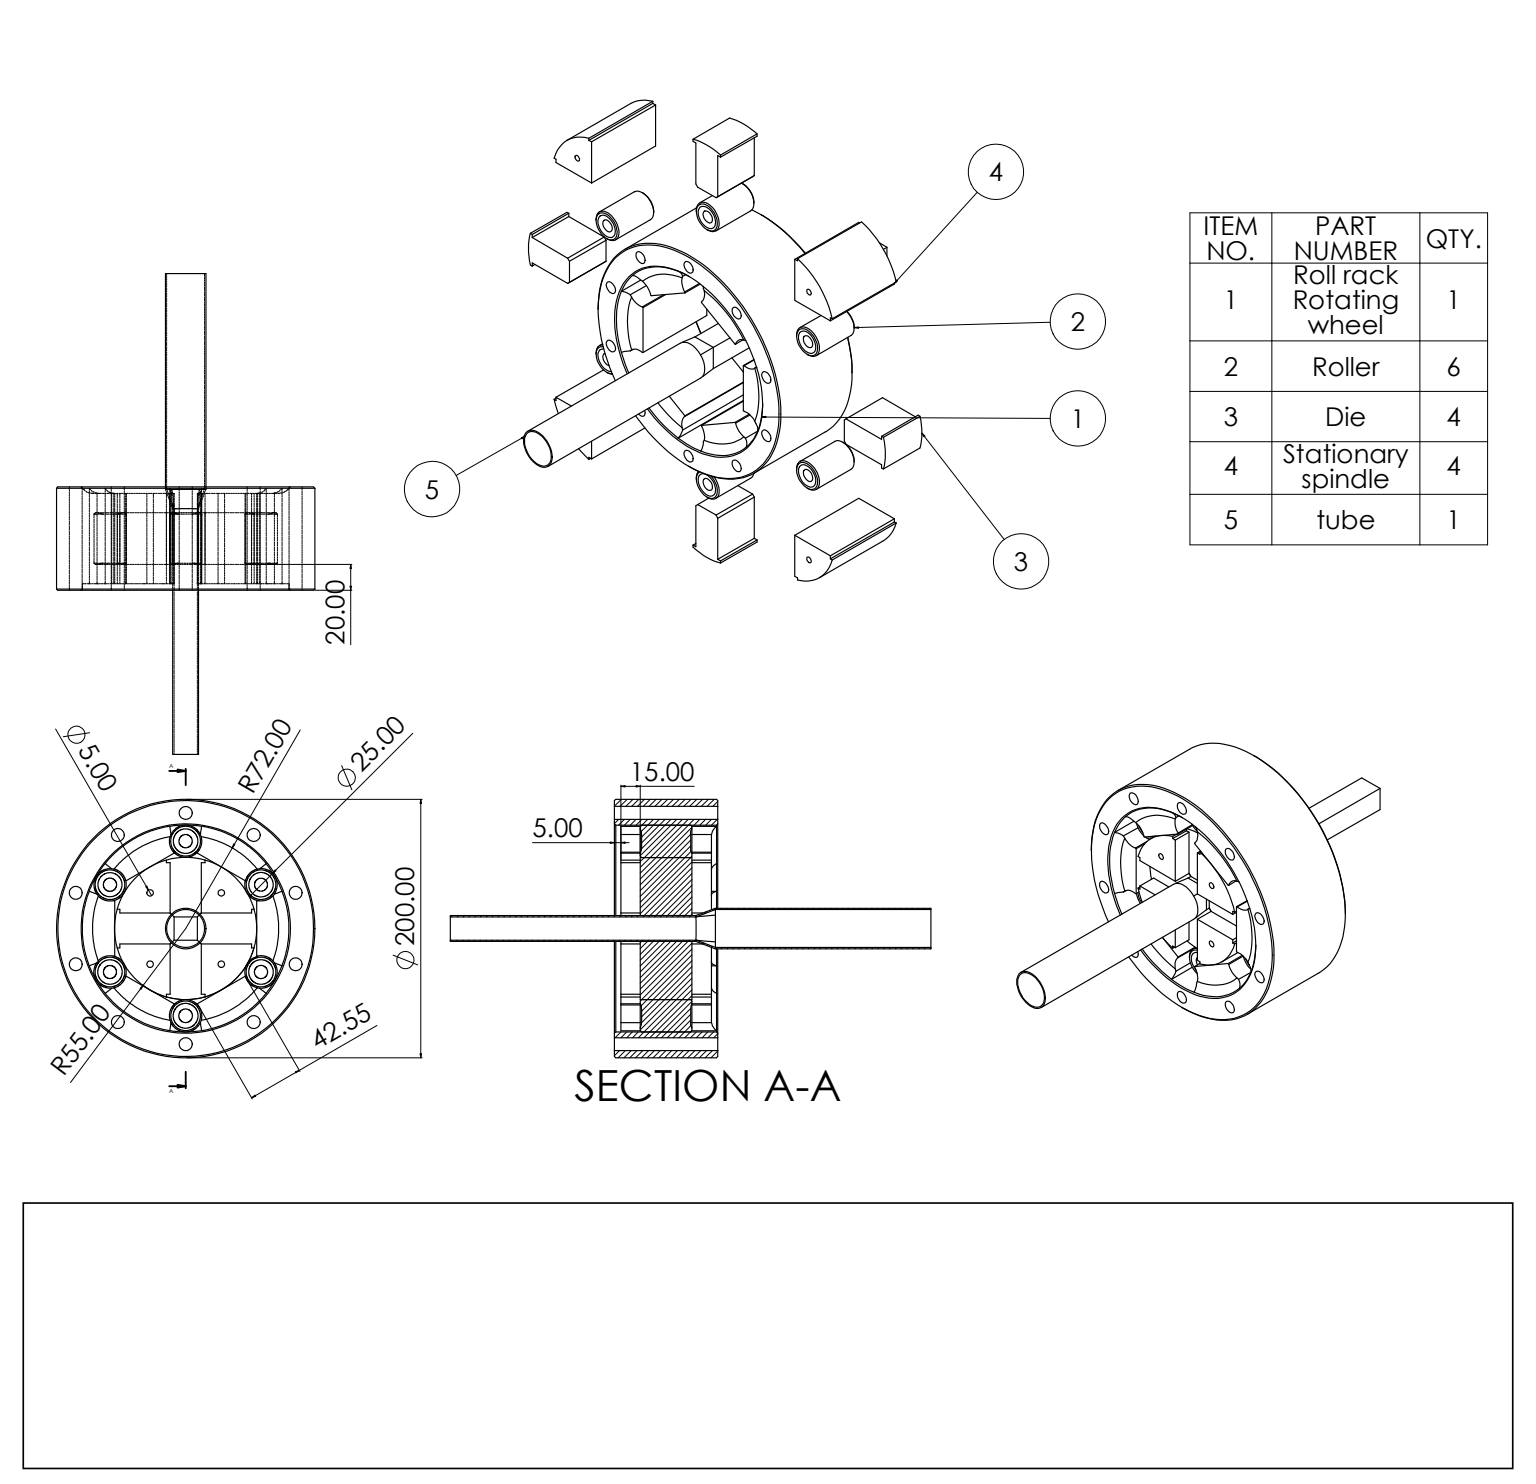
ISO-10303-21;
HEADER;
FILE_DESCRIPTION (('STEP AP214'),
    '1' );
FILE_NAME ('MAS-319',
    '2026-10-25T19:19:31',
    ( '' ),
    ( '' ),
    'SwSTEP 2.0',
    'SolidWorks 2025',
    '' );
FILE_SCHEMA (( 'AUTOMOTIVE_DESIGN' ));
ENDSEC;

DATA;
#1 = FACE_OUTER_BOUND ( 'NONE', #2199, .T. ) ;
#2 = AXIS2_PLACEMENT_3D ( 'NONE', #924, #2806, #4329 ) ;
#3 = CARTESIAN_POINT ( 'NONE',  ( 6.000509662810415534, -9.000000000000001776, 23.13502399099470708 ) ) ;
#4 = DIRECTION ( 'NONE',  ( 1.000000000000000000, 1.776356839400250465E-15, 0.000000000000000000 ) ) ;
#5 = ORIENTED_EDGE ( 'NONE', *, *, #469, .T. ) ;
#6 = LINE ( 'NONE', #939, #4428 ) ;
#7 = CYLINDRICAL_SURFACE ( 'NONE', #5135, 14.67638808697554964 ) ;
#8 = ADVANCED_FACE ( 'NONE', ( #6005 ), #1741, .T. ) ;
#9 = EDGE_CURVE ( 'NONE', #3175, #2261, #1933, .T. ) ;
#10 =( NAMED_UNIT ( * ) SI_UNIT ( $, .STERADIAN. ) SOLID_ANGLE_UNIT ( ) );
#11 = EDGE_LOOP ( 'NONE', ( #620, #96, #4571, #312 ) ) ;
#12 = DIRECTION ( 'NONE',  ( 0.6273063437270283149, 0.7787725926866119197, -0.000000000000000000 ) ) ;
#13 = PRODUCT_DEFINITION_SHAPE ( 'NONE', 'NONE',  #6150 ) ;
#14 = CARTESIAN_POINT ( 'NONE',  ( 4.154428044945162490, -8.963431230391421423, 23.04275563843252783 ) ) ;
#15 = VERTEX_POINT ( 'NONE', #3832 ) ;
#16 = ORIENTED_EDGE ( 'NONE', *, *, #1748, .F. ) ;
#17 = LINE ( 'NONE', #2869, #5066 ) ;
#18 = PLANE ( 'NONE',  #4619 ) ;
#19 =( NAMED_UNIT ( * ) SI_UNIT ( $, .STERADIAN. ) SOLID_ANGLE_UNIT ( ) );
#20 = DIRECTION ( 'NONE',  ( 2.553512956637860437E-15, -1.000000000000000000, 1.499031448860895265E-16 ) ) ;
#21 = EDGE_CURVE ( 'NONE', #4952, #1308, #564, .T. ) ;
#22 = CARTESIAN_POINT ( 'NONE',  ( 0.000000000000000000, 0.000000000000000000, -35.00000000000000000 ) ) ;
#23 = DIRECTION ( 'NONE',  ( 0.000000000000000000, -1.000000000000000000, 0.000000000000000000 ) ) ;
#24 = ORIENTED_EDGE ( 'NONE', *, *, #3439, .T. ) ;
#25 = CARTESIAN_POINT ( 'NONE',  ( 4.399209358691966720, 10.59950146047779995, 28.13666863833444154 ) ) ;
#26 = CARTESIAN_POINT ( 'NONE',  ( -0.8333333333332849646, 10.00000000000000000, 23.00000000000000355 ) ) ;
#27 = FACE_OUTER_BOUND ( 'NONE', #743, .T. ) ;
#28 = ORIENTED_EDGE ( 'NONE', *, *, #3600, .T. ) ;
#29 = CARTESIAN_POINT ( 'NONE',  ( -27.50000000000000355, -47.63139720814412215, 35.00000000000000000 ) ) ;
#30 = CARTESIAN_POINT ( 'NONE',  ( 0.000000000000000000, -67.50000000000000000, 35.00000000000000000 ) ) ;
#31 = CARTESIAN_POINT ( 'NONE',  ( -9.557272410707511767, 9.557272410707513544, 28.03893107092313031 ) ) ;
#32 = CARTESIAN_POINT ( 'NONE',  ( -68.69027832784050247, 26.57196568621489163, 35.13717928826310555 ) ) ;
#33 = ORIENTED_EDGE ( 'NONE', *, *, #1361, .F. ) ;
#34 = CARTESIAN_POINT ( 'NONE',  ( 0.000000000000000000, 0.000000000000000000, -39.00000000000002842 ) ) ;
#35 = DIRECTION ( 'NONE',  ( 0.000000000000000000, -1.000000000000000000, 0.000000000000000000 ) ) ;
#36 = DIRECTION ( 'NONE',  ( -0.000000000000000000, -0.000000000000000000, -1.000000000000000000 ) ) ;
#37 = VERTEX_POINT ( 'NONE', #2442 ) ;
#38 = CARTESIAN_POINT ( 'NONE',  ( 10.37777353962609972, -10.37777353962564852, 38.05103295300747845 ) ) ;
#39 = CARTESIAN_POINT ( 'NONE',  ( 5.954763795926170999, -9.638809746143389035, 25.54536317066256856 ) ) ;
#40 = APPLICATION_CONTEXT ( 'automotive_design' ) ;
#41 = EDGE_CURVE ( 'NONE', #1178, #2811, #1439, .T. ) ;
#42 = ORIENTED_EDGE ( 'NONE', *, *, #5266, .F. ) ;
#43 = ORIENTED_EDGE ( 'NONE', *, *, #3427, .F. ) ;
#44 = DIRECTION ( 'NONE',  ( 1.000000000000000000, 0.000000000000000000, 0.000000000000000000 ) ) ;
#45 = LINE ( 'NONE', #2928, #381 ) ;
#46 = DIRECTION ( 'NONE',  ( 5.551115123125782702E-17, 2.775557561562891351E-17, 1.000000000000000000 ) ) ;
#47 = CARTESIAN_POINT ( 'NONE',  ( 9.858401829237470437, -10.19494410001831142, 33.01259202755186095 ) ) ;
#48 = EDGE_CURVE ( 'NONE', #2705, #6084, #5252, .T. ) ;
#49 = ORIENTED_EDGE ( 'NONE', *, *, #1979, .T. ) ;
#50 = CARTESIAN_POINT ( 'NONE',  ( 1.902388932222473850, 12.74242197681752486, 33.26151580524048512 ) ) ;
#51 = CARTESIAN_POINT ( 'NONE',  ( 11.08488032081242380, 11.08488032081242025, 38.00000000000000000 ) ) ;
#52 = CARTESIAN_POINT ( 'NONE',  ( -85.08403291566554572, 27.64547812922971914, -40.00000000000000000 ) ) ;
#53 = AXIS2_PLACEMENT_3D ( 'NONE', #2121, #1570, #3471 ) ;
#54 = ORIENTED_EDGE ( 'NONE', *, *, #4887, .F. ) ;
#55 = DIRECTION ( 'NONE',  ( -0.000000000000000000, -0.000000000000000000, -1.000000000000000000 ) ) ;
#56 = ADVANCED_FACE ( 'NONE', ( #3401 ), #273, .T. ) ;
#57 = CARTESIAN_POINT ( 'NONE',  ( -10.12138240269938905, -10.27356722921338950, 35.55812462721154787 ) ) ;
#58 = AXIS2_PLACEMENT_3D ( 'NONE', #3243, #1826, #3726 ) ;
#59=STYLED_ITEM('',(#6177),#4119);
#60 = DIRECTION ( 'NONE',  ( -1.224646799147353207E-16, 1.000000000000000000, 0.000000000000000000 ) ) ;
#61 = PRODUCT_DEFINITION_SHAPE ( 'NONE', 'NONE',  #6146 ) ;
#62 = VECTOR ( 'NONE', #4313, 1000.000000000000000 ) ;
#63 = DIRECTION ( 'NONE',  ( 0.000000000000000000, 0.000000000000000000, -1.000000000000000000 ) ) ;
#64 = CARTESIAN_POINT ( 'NONE',  ( -3.819063922341606521, -14.20304409106748977, 38.16887386538299154 ) ) ;
#65 = AXIS2_PLACEMENT_3D ( 'NONE', #52, #3436, #1534 ) ;
#66 = ORIENTED_EDGE ( 'NONE', *, *, #1371, .T. ) ;
#67 = LINE ( 'NONE', #4284, #175 ) ;
#68 = AXIS2_PLACEMENT_3D ( 'NONE', #5525, #4167, #5643 ) ;
#69 = DIRECTION ( 'NONE',  ( -0.000000000000000000, 0.000000000000000000, 1.000000000000000000 ) ) ;
#70 = LINE ( 'NONE', #4287, #2332 ) ;
#71 = ORIENTED_EDGE ( 'NONE', *, *, #3542, .T. ) ;
#72 = LINE ( 'NONE', #3851, #3967 ) ;
#73 = AXIS2_PLACEMENT_3D ( 'NONE', #3304, #3763, #5645 ) ;
#74 = CARTESIAN_POINT ( 'NONE',  ( 3.019346778933465369, -14.42236408824967420, 38.33740271606986738 ) ) ;
#75 = MECHANICAL_DESIGN_GEOMETRIC_PRESENTATION_REPRESENTATION (  '', ( #2849 ), #6131 ) ;
#76 = ORIENTED_EDGE ( 'NONE', *, *, #3903, .F. ) ;
#77 = PRESENTATION_STYLE_ASSIGNMENT (( #649 ) ) ;
#78 = ORIENTED_EDGE ( 'NONE', *, *, #3494, .T. ) ;
#79 = DIRECTION ( 'NONE',  ( -0.000000000000000000, -0.000000000000000000, 1.000000000000000000 ) ) ;
#80 = DIRECTION ( 'NONE',  ( -0.000000000000000000, -0.000000000000000000, -1.000000000000000000 ) ) ;
#81 = CARTESIAN_POINT ( 'NONE',  ( 0.000000000000000000, 0.000000000000000000, 0.000000000000000000 ) ) ;
#82 = SHAPE_REPRESENTATION ( 'Roller', ( #73 ), #2452 ) ;
#83 = DIRECTION ( 'NONE',  ( 0.000000000000000000, 0.000000000000000000, 1.000000000000000000 ) ) ;
#84 = CARTESIAN_POINT ( 'NONE',  ( 58.45671475545002949, -33.74999999999933209, 35.00000000000000000 ) ) ;
#85 = ORIENTED_EDGE ( 'NONE', *, *, #1081, .T. ) ;
#86 = VECTOR ( 'NONE', #3244, 1000.000000000000114 ) ;
#87 = CARTESIAN_POINT ( 'NONE',  ( -1.016991241531515433, 14.74111653287705792, 38.35393095385146012 ) ) ;
#88 = CARTESIAN_POINT ( 'NONE',  ( -4.130675435985315210E-14, -1.067806758184287486E-13, -35.00000000000000000 ) ) ;
#89 = DIRECTION ( 'NONE',  ( -0.000000000000000000, -0.000000000000000000, 1.000000000000000000 ) ) ;
#90 = EDGE_CURVE ( 'NONE', #1861, #5383, #5968, .T. ) ;
#91 = ORIENTED_EDGE ( 'NONE', *, *, #553, .T. ) ;
#92 = CYLINDRICAL_SURFACE ( 'NONE', #5438, 12.50000000000000355 ) ;
#93 = CIRCLE ( 'NONE', #494, 100.0000000000000000 ) ;
#94 = DIRECTION ( 'NONE',  ( -0.000000000000000000, -0.000000000000000000, -1.000000000000000000 ) ) ;
#95 = VECTOR ( 'NONE', #4136, 1000.000000000000000 ) ;
#96 = ORIENTED_EDGE ( 'NONE', *, *, #2491, .F. ) ;
#97 = VECTOR ( 'NONE', #2993, 1000.000000000000000 ) ;
#98 = DIRECTION ( 'NONE',  ( -1.000000000000000000, 0.000000000000000000, 0.000000000000000000 ) ) ;
#99 = EDGE_CURVE ( 'NONE', #3250, #2370, #287, .T. ) ;
#100 = VECTOR ( 'NONE', #4962, 1000.000000000000000 ) ;
#101 = CARTESIAN_POINT ( 'NONE',  ( 0.000000000000000000, 67.50000000000000000, -20.00000000000000000 ) ) ;
#102 = CARTESIAN_POINT ( 'NONE',  ( 0.000000000000000000, 0.000000000000000000, 205.0000000000000568 ) ) ;
#103 = VERTEX_POINT ( 'NONE', #3026 ) ;
#104 = DIRECTION ( 'NONE',  ( 1.000000000000000000, 0.000000000000000000, 0.000000000000000000 ) ) ;
#105 = CARTESIAN_POINT ( 'NONE',  ( 0.000000000000000000, 0.000000000000000000, -20.00000000000000000 ) ) ;
#106 = CARTESIAN_POINT ( 'NONE',  ( 90.08403291566575888, -27.64547812922912939, -40.00000000000000000 ) ) ;
#107 = ORIENTED_EDGE ( 'NONE', *, *, #3615, .T. ) ;
#108 = CARTESIAN_POINT ( 'NONE',  ( 12.00000000000000000, 12.00000000000000355, 35.00000000000000000 ) ) ;
#109 = CARTESIAN_POINT ( 'NONE',  ( 6.925838250501021420, -10.16165675636470489, 28.06531976343184454 ) ) ;
#110 = ORIENTED_EDGE ( 'NONE', *, *, #2448, .F. ) ;
#111 = ORIENTED_EDGE ( 'NONE', *, *, #3009, .T. ) ;
#112 = DIRECTION ( 'NONE',  ( -1.000000000000000000, 0.000000000000000000, 0.000000000000000000 ) ) ;
#113 = LINE ( 'NONE', #4877, #5053 ) ;
#114 = DIRECTION ( 'NONE',  ( -6.989357705721002594E-18, 6.660920792866264645E-17, 1.000000000000000000 ) ) ;
#115 = CARTESIAN_POINT ( 'NONE',  ( -10.37777353962477278, -10.37777353962696303, 38.05103295300743582 ) ) ;
#116 = CARTESIAN_POINT ( 'NONE',  ( 10.38144361273100280, -10.38144361273100813, 38.10175261887127363 ) ) ;
#117 = ORIENTED_EDGE ( 'NONE', *, *, #561, .F. ) ;
#118 = PRODUCT_DEFINITION ( 'UNKNOWN', '', #4533, #1451 ) ;
#119 = ORIENTED_EDGE ( 'NONE', *, *, #3607, .F. ) ;
#120 = CARTESIAN_POINT ( 'NONE',  ( 4.273055220303958457, 9.778265677387498300, 25.59105958838677353 ) ) ;
#121 = CARTESIAN_POINT ( 'NONE',  ( 11.73806315776973719, 10.43169748385510687, 38.00000000000000000 ) ) ;
#122 = CARTESIAN_POINT ( 'NONE',  ( -13.19705249345109088, -6.492124056757525352, 38.13875458540262997 ) ) ;
#123 = ORIENTED_EDGE ( 'NONE', *, *, #596, .F. ) ;
#124 = CARTESIAN_POINT ( 'NONE',  ( 0.000000000000000000, 67.50000000000000000, -28.99999999999999645 ) ) ;
#125 = CARTESIAN_POINT ( 'NONE',  ( -11.58282027941458381, -3.645499761006322892, 30.69674202529823503 ) ) ;
#126 = ORIENTED_EDGE ( 'NONE', *, *, #1149, .F. ) ;
#127 = EDGE_CURVE ( 'NONE', #4172, #3364, #4015, .T. ) ;
#128 = EDGE_CURVE ( 'NONE', #3596, #4984, #485, .T. ) ;
#129 = CARTESIAN_POINT ( 'NONE',  ( 8.309552794738946702, -9.958856949317492990, 22.73823205004162773 ) ) ;
#130 = EDGE_CURVE ( 'NONE', #3466, #5138, #2058, .T. ) ;
#131 = CARTESIAN_POINT ( 'NONE',  ( 0.9493919581231019533, -14.67711297304296281, 38.18288466297301653 ) ) ;
#132 = VERTEX_POINT ( 'NONE', #187 ) ;
#133 = CARTESIAN_POINT ( 'NONE',  ( 6.000548030722291593, 8.999999999999994671, 23.13502304888907446 ) ) ;
#134 = CARTESIAN_POINT ( 'NONE',  ( 0.000000000000000000, 67.50000000000000000, -19.00000000000000711 ) ) ;
#135 = CARTESIAN_POINT ( 'NONE',  ( 11.82353433160363387, 71.60642589802917257, 35.00000000000000000 ) ) ;
#136 = CARTESIAN_POINT ( 'NONE',  ( -5.141101056459331353, 67.50000000000000000, -19.00000000000000000 ) ) ;
#137 = CARTESIAN_POINT ( 'NONE',  ( 8.328520801854331523, -12.11088206474084572, 38.20782360758020246 ) ) ;
#138 = EDGE_CURVE ( 'NONE', #2272, #193, #3964, .T. ) ;
#139 = ORIENTED_EDGE ( 'NONE', *, *, #5184, .F. ) ;
#140 = ORIENTED_EDGE ( 'NONE', *, *, #2807, .F. ) ;
#141 = DIRECTION ( 'NONE',  ( -1.000000000000000000, 0.000000000000000000, 0.000000000000000000 ) ) ;
#142 = DIRECTION ( 'NONE',  ( -0.4999999999999919509, -0.8660254037844432595, 0.000000000000000000 ) ) ;
#143 = DIRECTION ( 'NONE',  ( 0.8660254037844374864, 0.5000000000000018874, 0.000000000000000000 ) ) ;
#144 = CARTESIAN_POINT ( 'NONE',  ( 55.71784976887228424, -21.55374571496028224, -35.00000000000000000 ) ) ;
#145 = EDGE_LOOP ( 'NONE', ( #2402, #588 ) ) ;
#146 = CARTESIAN_POINT ( 'NONE',  ( 0.8581648076837656847, 9.928243323025451872, 25.63579099555280649 ) ) ;
#147 = CARTESIAN_POINT ( 'NONE',  ( 2.164213882025735280, 15.56315586465742484, 38.00000000000000711 ) ) ;
#148 = CARTESIAN_POINT ( 'NONE',  ( -99.00000000000005684, 0.000000000000000000, 40.00000000000000000 ) ) ;
#149 = VERTEX_POINT ( 'NONE', #4105 ) ;
#150 = DIRECTION ( 'NONE',  ( 0.000000000000000000, 0.000000000000000000, 1.000000000000000000 ) ) ;
#151 = CARTESIAN_POINT ( 'NONE',  ( -13.51119013911330491, -2.923529524533183821, 35.79437308157103814 ) ) ;
#152 = ORIENTED_EDGE ( 'NONE', *, *, #4059, .F. ) ;
#153 = CARTESIAN_POINT ( 'NONE',  ( -2.164213882025736613, -15.56315586465742484, 38.00000000000000711 ) ) ;
#154 = EDGE_CURVE ( 'NONE', #2132, #2202, #3672, .T. ) ;
#155 = CIRCLE ( 'NONE', #3811, 12.50000000000138733 ) ;
#156 = CARTESIAN_POINT ( 'NONE',  ( 8.964680801521355491, 2.491918585145397991, 23.07363600708416129 ) ) ;
#157 = CARTESIAN_POINT ( 'NONE',  ( -67.92475106770436355, 25.56373185532726566, 35.00000000000000000 ) ) ;
#158 = ORIENTED_EDGE ( 'NONE', *, *, #5715, .F. ) ;
#159 = FACE_OUTER_BOUND ( 'NONE', #3787, .T. ) ;
#160 = CIRCLE ( 'NONE', #3618, 5.000000000000004441 ) ;
#161 = APPLICATION_CONTEXT ( 'automotive_design' ) ;
#162 = CIRCLE ( 'NONE', #672, 99.00000000000005684 ) ;
#163 = LINE ( 'NONE', #3014, #5926 ) ;
#164 = EDGE_CURVE ( 'NONE', #4020, #3411, #5117, .T. ) ;
#165 = AXIS2_PLACEMENT_3D ( 'NONE', #2293, #4791, #5233 ) ;
#166 = CARTESIAN_POINT ( 'NONE',  ( -90.08403291566554572, 27.64547812922971914, 40.00000000000000000 ) ) ;
#167 = PRODUCT_DEFINITION_SHAPE ( 'NONE', 'NONE',  #6142 ) ;
#168 = CARTESIAN_POINT ( 'NONE',  ( 1.016991241531512769, -14.74111653287705792, 38.35393095385146012 ) ) ;
#169 = CIRCLE ( 'NONE', #2831, 12.49999999999999822 ) ;
#170 = AXIS2_PLACEMENT_3D ( 'NONE', #2221, #6035, #3192 ) ;
#171 = ORIENTED_EDGE ( 'NONE', *, *, #1511, .T. ) ;
#172 = FACE_OUTER_BOUND ( 'NONE', #5895, .T. ) ;
#173 = ORIENTED_EDGE ( 'NONE', *, *, #319, .F. ) ;
#174 = PLANE ( 'NONE',  #2670 ) ;
#175 = VECTOR ( 'NONE', #443, 1000.000000000000000 ) ;
#176 = B_SPLINE_CURVE_WITH_KNOTS ( 'NONE', 3,
 ( #5640, #360, #5088, #1772, #3271, #6050 ),
 .UNSPECIFIED., .F., .F.,
 ( 4, 2, 4 ),
 ( 2.991083261079382436E-05, 0.007589224902417026838, 0.01514853897222325982 ),
 .UNSPECIFIED. ) ;
#177 = DIRECTION ( 'NONE',  ( 0.000000000000000000, 0.000000000000000000, 1.000000000000000000 ) ) ;
#178 = SHAPE_DEFINITION_REPRESENTATION ( #473, #4081 ) ;
#179 = AXIS2_PLACEMENT_3D ( 'NONE', #1316, #5314, #565 ) ;
#180 = CARTESIAN_POINT ( 'NONE',  ( 8.999999999999998224, -9.999999999999998224, 23.00000000000000000 ) ) ;
#181 = EDGE_CURVE ( 'NONE', #882, #2297, #5215, .T. ) ;
#182 = DIRECTION ( 'NONE',  ( -0.000000000000000000, -0.000000000000000000, -1.000000000000000000 ) ) ;
#183 = ORIENTED_EDGE ( 'NONE', *, *, #3874, .T. ) ;
#184 = VECTOR ( 'NONE', #2953, 1000.000000000000000 ) ;
#185 = EDGE_LOOP ( 'NONE', ( #533, #4724, #4763, #1601 ) ) ;
#186 = CARTESIAN_POINT ( 'NONE',  ( 5.819377809724670669, 8.963566137365393871, 22.99383900881164067 ) ) ;
#187 = CARTESIAN_POINT ( 'NONE',  ( -11.33314185116896589, -72.77350886803867525, -35.00000000000000000 ) ) ;
#188 = FACE_OUTER_BOUND ( 'NONE', #757, .T. ) ;
#189 = AXIS2_PLACEMENT_3D ( 'NONE', #1496, #4390, #4322 ) ;
#190 = ORIENTED_EDGE ( 'NONE', *, *, #4573, .T. ) ;
#191 = DIRECTION ( 'NONE',  ( -1.000000000000000000, 0.000000000000000000, 0.000000000000000000 ) ) ;
#192 = CARTESIAN_POINT ( 'NONE',  ( -9.928243323025453648, 3.951802415609825688E-14, 25.63579099555280294 ) ) ;
#193 = VERTEX_POINT ( 'NONE', #6023 ) ;
#194 = CARTESIAN_POINT ( 'NONE',  ( -3.317157231508649495, -9.910574073276151807, 22.73823205004162773 ) ) ;
#195 = VECTOR ( 'NONE', #4584, 1000.000000000000000 ) ;
#196 = CARTESIAN_POINT ( 'NONE',  ( 13.51119013911330669, 2.923529524533184265, 35.79437308157104525 ) ) ;
#197 = AXIS2_PLACEMENT_3D ( 'NONE', #5583, #3182, #1309 ) ;
#198 = LINE ( 'NONE', #2374, #5423 ) ;
#199 = EDGE_LOOP ( 'NONE', ( #4634, #1674, #4035, #780 ) ) ;
#200 = CARTESIAN_POINT ( 'NONE',  ( -56.72666074499610289, 46.14586675604117971, 35.04915833130703362 ) ) ;
#201 = CIRCLE ( 'NONE', #4460, 80.99999999999998579 ) ;
#202 = AXIS2_PLACEMENT_3D ( 'NONE', #584, #4355, #522 ) ;
#203 = CARTESIAN_POINT ( 'NONE',  ( 0.8880320553140116369, -10.89081796499577237, 28.17941898721254645 ) ) ;
#204 = ORIENTED_EDGE ( 'NONE', *, *, #2780, .T. ) ;
#205 = DIRECTION ( 'NONE',  ( -0.000000000000000000, -0.000000000000000000, -1.000000000000000000 ) ) ;
#206 = ORIENTED_EDGE ( 'NONE', *, *, #6021, .F. ) ;
#207 = CARTESIAN_POINT ( 'NONE',  ( 14.30354638250598498, 3.321916882804190951, 38.17191617598167852 ) ) ;
#208 = EDGE_CURVE ( 'NONE', #3788, #4471, #2464, .T. ) ;
#209 = ADVANCED_FACE ( 'NONE', ( #3211 ), #1827, .F. ) ;
#210 = CARTESIAN_POINT ( 'NONE',  ( 85.08403291566575888, -27.64547812922912939, -79.99999999999998579 ) ) ;
#211 = APPLICATION_PROTOCOL_DEFINITION ( 'draft international standard', 'automotive_design', 1998, #2778 ) ;
#212 = VECTOR ( 'NONE', #3452, 1000.000000000000000 ) ;
#213 = LINE ( 'NONE', #3513, #2487 ) ;
#214 = DIRECTION ( 'NONE',  ( -0.1538769332794359124, -0.9880900209011910240, 0.000000000000000000 ) ) ;
#215 = EDGE_CURVE ( 'NONE', #764, #3704, #4242, .T. ) ;
#216 = ORIENTED_EDGE ( 'NONE', *, *, #469, .F. ) ;
#217 = ADVANCED_FACE ( 'NONE', ( #3609 ), #5647, .F. ) ;
#218 = CARTESIAN_POINT ( 'NONE',  ( 85.08403291566575888, -27.64547812922912939, -79.99999999999998579 ) ) ;
#219 = CARTESIAN_POINT ( 'NONE',  ( 9.999999999999998224, -9.999999999999998224, 23.00000000000000000 ) ) ;
#220 = CARTESIAN_POINT ( 'NONE',  ( 58.45671475545002949, -33.74999999999933209, -35.00000000000000000 ) ) ;
#221 = ORIENTED_EDGE ( 'NONE', *, *, #961, .T. ) ;
#222 = CARTESIAN_POINT ( 'NONE',  ( 0.000000000000000000, 67.50000000000000000, 35.00000000000000000 ) ) ;
#223 = CARTESIAN_POINT ( 'NONE',  ( -9.833810162157899271, -3.423816715609353079, 25.60794618818621160 ) ) ;
#224 = EDGE_LOOP ( 'NONE', ( #2924, #3585, #2921, #1569, #6030 ) ) ;
#225 = CARTESIAN_POINT ( 'NONE',  ( -8.999999999999998224, 8.999999999999998224, 23.00000000000000000 ) ) ;
#226 = CARTESIAN_POINT ( 'NONE',  ( 10.78034266696900012, 2.654236408786700085, 28.16346921039841789 ) ) ;
#227 = PLANE ( 'NONE',  #262 ) ;
#228 = EDGE_LOOP ( 'NONE', ( #2833, #2613, #5, #4505, #3148 ) ) ;
#229 = DIRECTION ( 'NONE',  ( -0.000000000000000000, -0.000000000000000000, 1.000000000000000000 ) ) ;
#230 = DIRECTION ( 'NONE',  ( 1.000000000000000000, 0.000000000000000000, 0.000000000000000000 ) ) ;
#231 = CARTESIAN_POINT ( 'NONE',  ( -4.003063095775588387, -14.21238549857230993, 38.32638145091770809 ) ) ;
#232 = ORIENTED_EDGE ( 'NONE', *, *, #1098, .F. ) ;
#233 = FACE_OUTER_BOUND ( 'NONE', #1137, .T. ) ;
#234 = ORIENTED_EDGE ( 'NONE', *, *, #392, .F. ) ;
#235 = CARTESIAN_POINT ( 'NONE',  ( 0.000000000000000000, 67.50000000000000000, 28.99999999999999645 ) ) ;
#236 = LINE ( 'NONE', #1613, #5345 ) ;
#237 = APPLICATION_PROTOCOL_DEFINITION ( 'draft international standard', 'automotive_design', 1998, #5772 ) ;
#238 = CARTESIAN_POINT ( 'NONE',  ( 0.000000000000000000, 0.000000000000000000, 45.00000000000000711 ) ) ;
#239 = CARTESIAN_POINT ( 'NONE',  ( -52.58482424179536707, 72.37680137756343868, 40.00000000000000000 ) ) ;
#240 = ORIENTED_EDGE ( 'NONE', *, *, #5458, .F. ) ;
#241 = EDGE_CURVE ( 'NONE', #1987, #2346, #2214, .T. ) ;
#242 = ORIENTED_EDGE ( 'NONE', *, *, #2892, .F. ) ;
#243 = CARTESIAN_POINT ( 'NONE',  ( 9.322893336083165394, 9.590870124851308631, 27.95908392747358562 ) ) ;
#244 = CARTESIAN_POINT ( 'NONE',  ( 9.916251082295017838, -4.147343260682193389, 22.73823205004162418 ) ) ;
#245 = PLANE ( 'NONE',  #776 ) ;
#246 = ORIENTED_EDGE ( 'NONE', *, *, #2518, .T. ) ;
#247 = PLANE ( 'NONE',  #2430 ) ;
#248 = EDGE_CURVE ( 'NONE', #5395, #3300, #425, .T. ) ;
#249 = MANIFOLD_SOLID_BREP ( 'Boss-Extrude4', #1653 ) ;
#250 = CARTESIAN_POINT ( 'NONE',  ( -10.32656711695238094, -6.095798759547100154, 28.09297316833070113 ) ) ;
#251 = VERTEX_POINT ( 'NONE', #3860 ) ;
#252 = DIRECTION ( 'NONE',  ( -0.000000000000000000, -0.000000000000000000, -1.000000000000000000 ) ) ;
#253 = EDGE_CURVE ( 'NONE', #2411, #1649, #3151, .T. ) ;
#254 = CARTESIAN_POINT ( 'NONE',  ( 10.46302782743270754, 5.247549479766026259, 28.11481907968152427 ) ) ;
#255 = LINE ( 'NONE', #729, #5225 ) ;
#256 = ORIENTED_EDGE ( 'NONE', *, *, #1736, .F. ) ;
#257 = ORIENTED_EDGE ( 'NONE', *, *, #4805, .F. ) ;
#258 = VECTOR ( 'NONE', #4022, 1000.000000000000000 ) ;
#259 = CARTESIAN_POINT ( 'NONE',  ( -5.685785403169735019, -12.74411457810409232, 35.74643938915854591 ) ) ;
#260 = ORIENTED_EDGE ( 'NONE', *, *, #822, .T. ) ;
#261 = LINE ( 'NONE', #1193, #1745 ) ;
#262 = AXIS2_PLACEMENT_3D ( 'NONE', #791, #5542, #322 ) ;
#263 = ORIENTED_EDGE ( 'NONE', *, *, #5260, .F. ) ;
#264 = CARTESIAN_POINT ( 'NONE',  ( -55.00000000000000711, -2.463307335887066074E-13, -35.00000000000000000 ) ) ;
#265 = COLOUR_RGB ( '',0.7921568627450980005, 0.8196078431372548767, 0.9333333333333333481 ) ;
#266 = DIRECTION ( 'NONE',  ( 0.000000000000000000, 0.000000000000000000, -1.000000000000000000 ) ) ;
#267 = FACE_OUTER_BOUND ( 'NONE', #1954, .T. ) ;
#268 = CARTESIAN_POINT ( 'NONE',  ( 58.45671475545002949, -33.74999999999933209, 35.00000000000000000 ) ) ;
#269 = AXIS2_PLACEMENT_3D ( 'NONE', #1659, #727, #3101 ) ;
#270 = AXIS2_PLACEMENT_3D ( 'NONE', #5191, #932, #5592 ) ;
#271 = ORIENTED_EDGE ( 'NONE', *, *, #5533, .F. ) ;
#272 = CARTESIAN_POINT ( 'NONE',  ( 7.487361748921665061, 8.967351122863068014, 22.92808036848186504 ) ) ;
#273 = B_SPLINE_SURFACE_WITH_KNOTS ( 'NONE', 3, 1, ( 
 ( #5313, #2482, #4370 ),
 ( #121, #3896, #1533 ),
 ( #3311, #5219, #957 ),
 ( #690, #3990, #1683 ),
 ( #2657, #4973, #3555 ),
 ( #774, #4553, #3001 ),
 ( #2602, #5904, #5405 ),
 ( #2062, #1619, #5435 ),
 ( #5474, #4431, #5936 ),
 ( #310, #2189, #4491 ),
 ( #5848, #4517, #1567 ),
 ( #745, #1230, #2626 ),
 ( #4940, #1174, #244 ),
 ( #2573, #1596, #3519 ),
 ( #3468, #3492, #5381 ),
 ( #1204, #1145, #5001 ),
 ( #4464, #1120, #3063 ),
 ( #2116, #219, #4911 ) ),
 .UNSPECIFIED., .F., .F., .F.,
 ( 4, 2, 2, 2, 2, 2, 2, 2, 4 ),
 ( 2, 1, 2 ),
 ( 0.000000000000000000, 0.1250000000000000000, 0.2500000000000000000, 0.3750000000000000000, 0.4999999999999999445, 0.6250000000000000000, 0.7500000000000000000, 0.8750000000000000000, 1.000000000000000000 ),
 ( 0.000000000000000000, 1.000000000000000000, 1.017451196663891722 ),
 .UNSPECIFIED. ) ;
#274 = DIRECTION ( 'NONE',  ( 0.000000000000000000, -1.000000000000000000, 0.000000000000000000 ) ) ;
#276 = AXIS2_PLACEMENT_3D ( 'NONE', #3833, #3374, #536 ) ;
#275 = CARTESIAN_POINT ( 'NONE',  ( -57.35713647666923976, 46.20154318182412112, -35.00000000000000000 ) ) ;
#277 = AXIS2_PLACEMENT_3D ( 'NONE', #5004, #3496, #662 ) ;
#278 = EDGE_LOOP ( 'NONE', ( #2591, #3538, #5453, #1395 ) ) ;
#279 = CARTESIAN_POINT ( 'NONE',  ( -99.00000000000000000, 1.218523565151616460E-14, -40.00000000000000000 ) ) ;
#280 = AXIS2_PLACEMENT_3D ( 'NONE', #4777, #4455, #2183 ) ;
#281 = CARTESIAN_POINT ( 'NONE',  ( -9.793760812180220654, 8.539139919159236314, 27.99841606626185353 ) ) ;
#282 = ORIENTED_EDGE ( 'NONE', *, *, #3578, .T. ) ;
#283 = AXIS2_PLACEMENT_3D ( 'NONE', #2617, #2590, #2677 ) ;
#284 = PLANE ( 'NONE',  #4114 ) ;
#285 = EDGE_CURVE ( 'NONE', #1194, #1920, #2836, .T. ) ;
#286 = FACE_OUTER_BOUND ( 'NONE', #5823, .T. ) ;
#287 = CIRCLE ( 'NONE', #788, 80.00000000000000000 ) ;
#288 = FACE_OUTER_BOUND ( 'NONE', #4896, .T. ) ;
#289 = DIRECTION ( 'NONE',  ( -0.000000000000000000, -0.000000000000000000, -1.000000000000000000 ) ) ;
#290 = ORIENTED_EDGE ( 'NONE', *, *, #3576, .F. ) ;
#291 = ORIENTED_EDGE ( 'NONE', *, *, #9, .T. ) ;
#292 = ADVANCED_FACE ( 'NONE', ( #988 ), #5742, .F. ) ;
#293 = VECTOR ( 'NONE', #3601, 1000.000000000000000 ) ;
#294 = CARTESIAN_POINT ( 'NONE',  ( 2.830884587392746621, -12.60026679007841466, 33.25110354061416018 ) ) ;
#295 = ORIENTED_EDGE ( 'NONE', *, *, #6012, .F. ) ;
#296 = CARTESIAN_POINT ( 'NONE',  ( -11.50000000000000355, 67.50000000000000000, 20.00000000000000000 ) ) ;
#297 = VECTOR ( 'NONE', #4183, 1000.000000000000000 ) ;
#298 = ORIENTED_EDGE ( 'NONE', *, *, #2594, .T. ) ;
#299 = PLANE ( 'NONE',  #2579 ) ;
#300 = CARTESIAN_POINT ( 'NONE',  ( 57.35713647667095927, 46.20154318182582642, 35.00000000000000000 ) ) ;
#301 = APPLICATION_PROTOCOL_DEFINITION ( 'draft international standard', 'automotive_design', 1998, #2134 ) ;
#302 = AXIS2_PLACEMENT_3D ( 'NONE', #2834, #4360, #112 ) ;
#303 = CARTESIAN_POINT ( 'NONE',  ( 15.67638808697555142, 1.919803849290630886E-15, 205.0000000000000568 ) ) ;
#304 = CARTESIAN_POINT ( 'NONE',  ( -9.999999999999998224, 1.666666666666715368, 23.00000000000000000 ) ) ;
#305 = AXIS2_PLACEMENT_3D ( 'NONE', #991, #5469, #718 ) ;
#306 = ORIENTED_EDGE ( 'NONE', *, *, #668, .F. ) ;
#307 = LINE ( 'NONE', #5608, #5057 ) ;
#308 = DIRECTION ( 'NONE',  ( 1.000000000000000000, 0.000000000000000000, 0.000000000000000000 ) ) ;
#309 = CIRCLE ( 'NONE', #2876, 12.49999999999999822 ) ;
#310 = CARTESIAN_POINT ( 'NONE',  ( 15.67638808697555142, -1.082228759108216254, 38.00000000000000711 ) ) ;
#311 = DIRECTION ( 'NONE',  ( -0.7787725926866080339, -0.6273063437270329779, 0.000000000000000000 ) ) ;
#312 = ORIENTED_EDGE ( 'NONE', *, *, #2008, .T. ) ;
#313 = PRODUCT_DEFINITION ( 'UNKNOWN', '', #4945, #1510 ) ;
#314 = CARTESIAN_POINT ( 'NONE',  ( 8.964120815521452457, -3.322922547535530846, 23.06129036953744915 ) ) ;
#315 = CARTESIAN_POINT ( 'NONE',  ( -10.78034266696900190, 2.654236408786762702, 28.16346921039841078 ) ) ;
#316 = ORIENTED_EDGE ( 'NONE', *, *, #3343, .F. ) ;
#317 = CARTESIAN_POINT ( 'NONE',  ( -10.08321815271042432, 9.378998278013591872, 27.91486726096250948 ) ) ;
#318 = CARTESIAN_POINT ( 'NONE',  ( 0.000000000000000000, 67.50000000000000000, -19.00000000000000711 ) ) ;
#319 = EDGE_CURVE ( 'NONE', #3286, #747, #5307, .T. ) ;
#320 = EDGE_CURVE ( 'NONE', #1017, #4020, #950, .T. ) ;
#321 = DIRECTION ( 'NONE',  ( 1.000000000000000000, 8.673617379884026597E-16, -0.000000000000000000 ) ) ;
#322 = DIRECTION ( 'NONE',  ( -0.9326495259660518844, 0.3607836771741465554, 0.000000000000000000 ) ) ;
#323 = EDGE_LOOP ( 'NONE', ( #4367, #5379, #3695, #5284 ) ) ;
#324 = EDGE_CURVE ( 'NONE', #559, #1473, #4803, .T. ) ;
#325 = CARTESIAN_POINT ( 'NONE',  ( -6.737147714782520502, -13.11522978513662530, 38.26633100282688105 ) ) ;
#326 = ORIENTED_EDGE ( 'NONE', *, *, #3380, .T. ) ;
#327 = DIRECTION ( 'NONE',  ( 0.000000000000000000, 0.000000000000000000, 1.000000000000000000 ) ) ;
#328 = VERTEX_POINT ( 'NONE', #555 ) ;
#329 = PLANE ( 'NONE',  #2861 ) ;
#330 = PLANE ( 'NONE',  #3954 ) ;
#331 = ITEM_DEFINED_TRANSFORMATION ( 'NONE', 'NONE', #2745,  #73 ) ;
#332 = LINE ( 'NONE', #833, #5327 ) ;
#333 = CARTESIAN_POINT ( 'NONE',  ( -13.97471987708211216, -7.178663235509280760, 37.99999999999999289 ) ) ;
#334 = EDGE_CURVE ( 'NONE', #2774, #836, #5704, .T. ) ;
#335 = CARTESIAN_POINT ( 'NONE',  ( -45.92560378283280187, -36.99336990414421678, 35.00000000000000000 ) ) ;
#336 = EDGE_LOOP ( 'NONE', ( #5694, #5269, #1258, #942 ) ) ;
#337 = CARTESIAN_POINT ( 'NONE',  ( -80.00000000000000000, 9.858406733136196781E-15, 38.99999999999995737 ) ) ;
#338 = DIRECTION ( 'NONE',  ( -0.000000000000000000, -0.000000000000000000, -1.000000000000000000 ) ) ;
#339 = DIRECTION ( 'NONE',  ( 0.8660254037844374864, 0.5000000000000018874, 0.000000000000000000 ) ) ;
#340 =( NAMED_UNIT ( * ) PLANE_ANGLE_UNIT ( ) SI_UNIT ( $, .RADIAN. ) );
#341 = CARTESIAN_POINT ( 'NONE',  ( 8.965240787521256749, -1.660914622755447212, 23.08598164463087343 ) ) ;
#342 = CARTESIAN_POINT ( 'NONE',  ( -11.98089146579573061, 5.533593864557679431, 33.20390238845318720 ) ) ;
#343 = ORIENTED_EDGE ( 'NONE', *, *, #4753, .T. ) ;
#344 = CARTESIAN_POINT ( 'NONE',  ( -8.662324224478984647, 10.23352841777492017, 30.54531597708798074 ) ) ;
#345 = DIRECTION ( 'NONE',  ( 0.4999999999999979461, 0.8660254037844397068, 0.000000000000000000 ) ) ;
#346 = CARTESIAN_POINT ( 'NONE',  ( 0.000000000000000000, 0.000000000000000000, -35.00000000000000000 ) ) ;
#347 = CARTESIAN_POINT ( 'NONE',  ( 80.00000000000000000, 9.797174393178826052E-15, -35.00000000000000000 ) ) ;
#348 = DIRECTION ( 'NONE',  ( 0.9326495259660493309, -0.3607836771741531612, 0.000000000000000000 ) ) ;
#349 = EDGE_LOOP ( 'NONE', ( #4550, #1268, #2494, #2612 ) ) ;
#350 = EDGE_CURVE ( 'NONE', #4063, #382, #1866, .T. ) ;
#351 = CARTESIAN_POINT ( 'NONE',  ( -8.539139919159234537, -9.793760812180220654, 27.99841606626185353 ) ) ;
#352 = ORIENTED_EDGE ( 'NONE', *, *, #5211, .T. ) ;
#353 = CARTESIAN_POINT ( 'NONE',  ( 10.37777353962609972, -10.37777353962564852, 38.05103295300747845 ) ) ;
#354 = VERTEX_POINT ( 'NONE', #4776 ) ;
#355 = LINE ( 'NONE', #765, #5264 ) ;
#356 = LINE ( 'NONE', #854, #4752 ) ;
#357 = ADVANCED_FACE ( 'NONE', ( #528 ), #1432, .F. ) ;
#358 = CYLINDRICAL_SURFACE ( 'NONE', #2932, 5.000000000000005329 ) ;
#359 = CARTESIAN_POINT ( 'NONE',  ( -9.916251082295017838, 4.147343260682193389, 22.73823205004162418 ) ) ;
#360 = CARTESIAN_POINT ( 'NONE',  ( 10.19629538392542933, -10.19629538388540446, 35.54424335298407556 ) ) ;
#361 = CIRCLE ( 'NONE', #2438, 5.000000000000003553 ) ;
#362 = EDGE_LOOP ( 'NONE', ( #5160, #1425, #4288, #5479, #680 ) ) ;
#363 = PLANE ( 'NONE',  #2855 ) ;
#364 = CYLINDRICAL_SURFACE ( 'NONE', #2030, 5.000000000000004441 ) ;
#365 = CARTESIAN_POINT ( 'NONE',  ( 2.411881101062863575, 14.48475173028204566, 38.17746263717076971 ) ) ;
#366 = EDGE_CURVE ( 'NONE', #3309, #2604, #45, .T. ) ;
#367 = VECTOR ( 'NONE', #4179, 1000.000000000000000 ) ;
#368 =( REPRESENTATION_RELATIONSHIP ('NONE','NONE', #4716, #82 ) REPRESENTATION_RELATIONSHIP_WITH_TRANSFORMATION ( #4933 )SHAPE_REPRESENTATION_RELATIONSHIP( ) );
#369 = CARTESIAN_POINT ( 'NONE',  ( 12.81596724893641515, -0.9505942623812210224, 33.26667497053200151 ) ) ;
#370 = CARTESIAN_POINT ( 'NONE',  ( -8.963566137365393871, 5.819377809724669781, 22.99383900881164067 ) ) ;
#371 = AXIS2_PLACEMENT_3D ( 'NONE', #5124, #1347, #5615 ) ;
#372 = ORIENTED_EDGE ( 'NONE', *, *, #1885, .T. ) ;
#373 = AXIS2_PLACEMENT_3D ( 'NONE', #5753, #1444, #5257 ) ;
#374 = CARTESIAN_POINT ( 'NONE',  ( -2.035738251814317223, 14.63232105816060979, 38.34842656511671066 ) ) ;
#375 = DIRECTION ( 'NONE',  ( 0.1538769332794487910, -0.9880900209011889146, 0.000000000000000000 ) ) ;
#376 = CYLINDRICAL_SURFACE ( 'NONE', #2340, 2.499999999999998668 ) ;
#377 = AXIS2_PLACEMENT_3D ( 'NONE', #1815, #1301, #327 ) ;
#378 = DIRECTION ( 'NONE',  ( 0.9880900209011890256, 0.1538769332794488465, -0.000000000000000000 ) ) ;
#379 = CARTESIAN_POINT ( 'NONE',  ( -1.131281550719566266E-13, -1.761763928569765259E-14, -35.00000000000000000 ) ) ;
#380 = CARTESIAN_POINT ( 'NONE',  ( -9.419333092093008730, -9.933255351449998827, 30.50691708577706152 ) ) ;
#381 = VECTOR ( 'NONE', #2434, 1000.000000000000000 ) ;
#382 = VERTEX_POINT ( 'NONE', #5209 ) ;
#383 = FACE_OUTER_BOUND ( 'NONE', #5206, .T. ) ;
#384 = ORIENTED_EDGE ( 'NONE', *, *, #2250, .F. ) ;
#385 = DIRECTION ( 'NONE',  ( 0.4999999999999980016, 0.8660254037844398178, 0.000000000000000000 ) ) ;
#386 = DIRECTION ( 'NONE',  ( 0.7071067811865474617, 8.659560562354932858E-17, -0.7071067811865474617 ) ) ;
#387 = CARTESIAN_POINT ( 'NONE',  ( 0.000000000000000000, 0.000000000000000000, -35.00000000000000000 ) ) ;
#388 = CARTESIAN_POINT ( 'NONE',  ( -9.999999999999998224, 6.666666666666692720, 23.00000000000000000 ) ) ;
#389 = CIRCLE ( 'NONE', #3743, 81.00000000000004263 ) ;
#390 = CARTESIAN_POINT ( 'NONE',  ( -46.52501622030417394, 37.47620048660903080, -35.00000000000000000 ) ) ;
#391 = ADVANCED_FACE ( 'NONE', ( #4837 ), #4296, .F. ) ;
#392 = EDGE_CURVE ( 'NONE', #6119, #506, #4546, .T. ) ;
#393 = CIRCLE ( 'NONE', #4250, 5.000000000000004441 ) ;
#394 = ORIENTED_EDGE ( 'NONE', *, *, #319, .T. ) ;
#395 = FACE_OUTER_BOUND ( 'NONE', #5732, .T. ) ;
#396 = CARTESIAN_POINT ( 'NONE',  ( 45.92560378283280187, 36.99336990414421678, 35.00000000000000000 ) ) ;
#397 =( NAMED_UNIT ( * ) PLANE_ANGLE_UNIT ( ) SI_UNIT ( $, .RADIAN. ) );
#398 = AXIS2_PLACEMENT_3D ( 'NONE', #2597, #2507, #3090 ) ;
#399 = CARTESIAN_POINT ( 'NONE',  ( 14.63234267792704557, -2.035630462091353898, 38.34842398122204798 ) ) ;
#400 = AXIS2_PLACEMENT_3D ( 'NONE', #1642, #1196, #3511 ) ;
#401 = EDGE_CURVE ( 'NONE', #3704, #1698, #113, .T. ) ;
#402 = CARTESIAN_POINT ( 'NONE',  ( -9.908812303639313868, 1.716658579843643118, 25.63028407385522911 ) ) ;
#403 = VECTOR ( 'NONE', #3278, 1000.000000000000000 ) ;
#404 = VERTEX_POINT ( 'NONE', #2337 ) ;
#405 = CARTESIAN_POINT ( 'NONE',  ( -8.321944142006520551, 8.970286642449650572, 22.89273687632151066 ) ) ;
#406 = CARTESIAN_POINT ( 'NONE',  ( 57.35713647666955950, -46.20154318182373032, 35.13717928826270054 ) ) ;
#407 = ORIENTED_EDGE ( 'NONE', *, *, #3155, .F. ) ;
#408 = CARTESIAN_POINT ( 'NONE',  ( -47.58482424179695158, -72.37680137756228760, -79.99999999999998579 ) ) ;
#409 = EDGE_CURVE ( 'NONE', #4283, #4835, #4739, .T. ) ;
#410 = CARTESIAN_POINT ( 'NONE',  ( 45.92560378283317135, -36.99336990414376913, -35.00000000000000000 ) ) ;
#411 = LINE ( 'NONE', #2288, #367 ) ;
#412 = CARTESIAN_POINT ( 'NONE',  ( -8.926511697459380557, -11.12726264164139600, 35.63515070857870626 ) ) ;
#413 = VERTEX_POINT ( 'NONE', #3086 ) ;
#414 = DIRECTION ( 'NONE',  ( 8.673617379883998001E-16, 1.000000000000000000, 0.000000000000000000 ) ) ;
#415 = EDGE_LOOP ( 'NONE', ( #3992, #873, #2536, #5412 ) ) ;
#416 = CARTESIAN_POINT ( 'NONE',  ( -15.00000000000000178, 52.91502622129182498, -20.00000000000000000 ) ) ;
#417 = CARTESIAN_POINT ( 'NONE',  ( -54.99999999999990052, -21.27605460800010206, 35.00000000000000000 ) ) ;
#418 = CARTESIAN_POINT ( 'NONE',  ( 0.000000000000000000, 0.000000000000000000, 38.99999999999995737 ) ) ;
#419 = ORIENTED_EDGE ( 'NONE', *, *, #6088, .T. ) ;
#420 = CARTESIAN_POINT ( 'NONE',  ( -13.47611570251764590, -8.069545871843427420, 37.99999999999998579 ) ) ;
#421 = DIRECTION ( 'NONE',  ( 0.000000000000000000, 0.000000000000000000, 1.000000000000000000 ) ) ;
#422 = ORIENTED_EDGE ( 'NONE', *, *, #959, .T. ) ;
#423 = CARTESIAN_POINT ( 'NONE',  ( -9.999999999999998224, -9.999999999999998224, 23.00000000000000000 ) ) ;
#424 = DIRECTION ( 'NONE',  ( -0.000000000000000000, -0.000000000000000000, -1.000000000000000000 ) ) ;
#425 = LINE ( 'NONE', #3727, #495 ) ;
#426 = ADVANCED_FACE ( 'NONE', ( #4483 ), #2145, .F. ) ;
#427 = CARTESIAN_POINT ( 'NONE',  ( 11.85339260696609109, 0.9193131588475963456, 30.72304697887226510 ) ) ;
#428 = CARTESIAN_POINT ( 'NONE',  ( 0.000000000000000000, -67.50000000000000000, 35.00000000000000000 ) ) ;
#429 = VERTEX_POINT ( 'NONE', #3953 ) ;
#430 = CARTESIAN_POINT ( 'NONE',  ( -5.685785403169716368, 12.74411457810409587, 35.74643938915853880 ) ) ;
#431 = LINE ( 'NONE', #905, #1941 ) ;
#432 = EDGE_CURVE ( 'NONE', #3051, #2891, #3112, .T. ) ;
#433 = ADVANCED_FACE ( 'NONE', ( #2109 ), #652, .T. ) ;
#434 = ORIENTED_EDGE ( 'NONE', *, *, #2926, .T. ) ;
#435 = DIRECTION ( 'NONE',  ( 0.4999999999999980571, 0.8660254037844398178, 0.000000000000000000 ) ) ;
#436 = CARTESIAN_POINT ( 'NONE',  ( -10.63625351335941538, -9.632247231687289357, 35.59852902770368388 ) ) ;
#437 = CARTESIAN_POINT ( 'NONE',  ( -14.67638808697506114, 0.4806947631990008407, 38.18288438803430296 ) ) ;
#438 = EDGE_CURVE ( 'NONE', #2727, #2151, #236, .T. ) ;
#439 = CARTESIAN_POINT ( 'NONE',  ( 0.000000000000000000, 0.000000000000000000, 40.00000000000000000 ) ) ;
#440 = ORIENTED_EDGE ( 'NONE', *, *, #2522, .F. ) ;
#441 = CARTESIAN_POINT ( 'NONE',  ( -9.192833548570002122, 59.02994620156853500, 35.00000000000000000 ) ) ;
#442 = ORIENTED_EDGE ( 'NONE', *, *, #4598, .F. ) ;
#443 = DIRECTION ( 'NONE',  ( -0.000000000000000000, -0.000000000000000000, -1.000000000000000000 ) ) ;
#444 = LINE ( 'NONE', #1490, #3945 ) ;
#445 = SURFACE_SIDE_STYLE ('',( #2827 ) ) ;
#446 = ORIENTED_EDGE ( 'NONE', *, *, #3414, .T. ) ;
#447 = DIRECTION ( 'NONE',  ( -0.9326495259660493309, 0.3607836771741531612, 0.000000000000000000 ) ) ;
#448 = CARTESIAN_POINT ( 'NONE',  ( 0.000000000000000000, 0.000000000000000000, 39.00000000000007105 ) ) ;
#449 = ORIENTED_EDGE ( 'NONE', *, *, #4908, .F. ) ;
#450 = ORIENTED_EDGE ( 'NONE', *, *, #856, .T. ) ;
#451 = CARTESIAN_POINT ( 'NONE',  ( -10.00000000000000178, 10.00000000000000178, -20.00000000000000000 ) ) ;
#452 = FACE_OUTER_BOUND ( 'NONE', #336, .T. ) ;
#453 = CARTESIAN_POINT ( 'NONE',  ( -0.9493919581226956117, 14.67711297304298768, 38.18288466297298811 ) ) ;
#454 = CARTESIAN_POINT ( 'NONE',  ( 67.15076586955507310, 25.97642475654038208, 45.00000000000000711 ) ) ;
#455 = DIRECTION ( 'NONE',  ( -0.000000000000000000, -0.000000000000000000, -1.000000000000000000 ) ) ;
#456 = VECTOR ( 'NONE', #3870, 1000.000000000000000 ) ;
#457 = ORIENTED_EDGE ( 'NONE', *, *, #2284, .T. ) ;
#458 = CARTESIAN_POINT ( 'NONE',  ( -3.423816715609354411, 9.833810162157899271, 25.60794618818621160 ) ) ;
#459 = PRODUCT_DEFINITION_SHAPE ( 'NONE', 'NONE',  #6156 ) ;
#460 = ORIENTED_EDGE ( 'NONE', *, *, #2064, .F. ) ;
#462 = CIRCLE ( 'NONE', #5923, 10.00000000000000000 ) ;
#461 = DIRECTION ( 'NONE',  ( -0.1538769332794359124, -0.9880900209011910240, 0.000000000000000000 ) ) ;
#463 = CIRCLE ( 'NONE', #5827, 80.00000000000000000 ) ;
#464 = VERTEX_POINT ( 'NONE', #2022 ) ;
#465 = CARTESIAN_POINT ( 'NONE',  ( 0.000000000000000000, 0.000000000000000000, 40.00000000000000000 ) ) ;
#466 = VECTOR ( 'NONE', #2853, 1000.000000000000000 ) ;
#467 = CARTESIAN_POINT ( 'NONE',  ( -8.983694681928700021, -9.994658916190591214, 22.80938439471025703 ) ) ;
#468 = ADVANCED_FACE ( 'NONE', ( #2082, #5872 ), #4008, .T. ) ;
#469 = EDGE_CURVE ( 'NONE', #4283, #4976, #5856, .T. ) ;
#470 = CARTESIAN_POINT ( 'NONE',  ( 57.35713647667095927, 46.20154318182582642, -35.00000000000000000 ) ) ;
#471 = AXIS2_PLACEMENT_3D ( 'NONE', #3650, #3190, #2720 ) ;
#472 = CIRCLE ( 'NONE', #5133, 5.000000000000004441 ) ;
#473 = PRODUCT_DEFINITION_SHAPE ( 'NONE', 'NONE',  #5093 ) ;
#474 = CARTESIAN_POINT ( 'NONE',  ( 46.52501622030217021, 37.47620048660763103, 35.00000000000000000 ) ) ;
#475 = AXIS2_PLACEMENT_3D ( 'NONE', #1088, #2025, #3550 ) ;
#476 = ADVANCED_FACE ( 'NONE', ( #3547 ), #1167, .F. ) ;
#477 = ORIENTED_EDGE ( 'NONE', *, *, #4239, .T. ) ;
#478 = DIRECTION ( 'NONE',  ( 0.000000000000000000, 0.000000000000000000, 1.000000000000000000 ) ) ;
#479 = ORIENTED_EDGE ( 'NONE', *, *, #2367, .F. ) ;
#480 = CIRCLE ( 'NONE', #3045, 5.000000000000004441 ) ;
#481 = LINE ( 'NONE', #2362, #700 ) ;
#482 = CYLINDRICAL_SURFACE ( 'NONE', #4115, 12.49999999999999822 ) ;
#483 = ORIENTED_EDGE ( 'NONE', *, *, #1361, .T. ) ;
#484 = LINE ( 'NONE', #4827, #2071 ) ;
#485 = CIRCLE ( 'NONE', #982, 12.50000000000138556 ) ;
#486 = CARTESIAN_POINT ( 'NONE',  ( 5.533593864557655451, -11.98089146579573061, 33.20390238845318720 ) ) ;
#487 = APPLICATION_CONTEXT ( 'automotive_design' ) ;
#488 = EDGE_LOOP ( 'NONE', ( #3553, #1325 ) ) ;
#489 = ORIENTED_EDGE ( 'NONE', *, *, #127, .F. ) ;
#490 = FACE_OUTER_BOUND ( 'NONE', #2075, .T. ) ;
#491 = DIRECTION ( 'NONE',  ( 0.7787725926866119197, -0.6273063437270283149, 0.000000000000000000 ) ) ;
#492 = CARTESIAN_POINT ( 'NONE',  ( -55.71784976887420271, -21.55374571496209057, 35.00000000000000000 ) ) ;
#493 = DIRECTION ( 'NONE',  ( 0.000000000000000000, -5.551115123125782702E-17, 1.000000000000000000 ) ) ;
#494 = AXIS2_PLACEMENT_3D ( 'NONE', #1360, #5019, #5052 ) ;
#495 = VECTOR ( 'NONE', #5181, 1000.000000000000000 ) ;
#496 = DIRECTION ( 'NONE',  ( -0.000000000000000000, -0.000000000000000000, 1.000000000000000000 ) ) ;
#497 = CARTESIAN_POINT ( 'NONE',  ( 9.590870124851305079, -9.322893336083168947, 27.95908392747358562 ) ) ;
#498 = VECTOR ( 'NONE', #1818, 1000.000000000000000 ) ;
#499 = ORIENTED_EDGE ( 'NONE', *, *, #5572, .F. ) ;
#500 = CARTESIAN_POINT ( 'NONE',  ( 4.003063095775587499, 14.21238549857231170, 38.32638145091770809 ) ) ;
#501 = AXIS2_PLACEMENT_3D ( 'NONE', #5606, #4101, #6017 ) ;
#502 = CARTESIAN_POINT ( 'NONE',  ( 0.8333333333333816650, 9.999999999999998224, 23.00000000000000000 ) ) ;
#503 = DIRECTION ( 'NONE',  ( 4.496403249731883200E-15, -1.000000000000000000, 0.000000000000000000 ) ) ;
#504 = EDGE_CURVE ( 'NONE', #1915, #1987, #3073, .T. ) ;
#505 = CIRCLE ( 'NONE', #3166, 10.00000000000000178 ) ;
#506 = VERTEX_POINT ( 'NONE', #1560 ) ;
#507 = DIRECTION ( 'NONE',  ( -0.000000000000000000, -0.000000000000000000, -1.000000000000000000 ) ) ;
#508 = CIRCLE ( 'NONE', #5964, 12.50000000000000355 ) ;
#509 = CARTESIAN_POINT ( 'NONE',  ( 50.91502622129181788, 0.000000000000000000, 35.00000000000000000 ) ) ;
#510 = CYLINDRICAL_SURFACE ( 'NONE', #4830, 12.49999999999999822 ) ;
#511 = AXIS2_PLACEMENT_3D ( 'NONE', #4477, #2587, #1635 ) ;
#512 = ADVANCED_FACE ( 'NONE', ( #3981 ), #3487, .F. ) ;
#513 = EDGE_CURVE ( 'NONE', #2290, #1698, #4659, .T. ) ;
#514 = CARTESIAN_POINT ( 'NONE',  ( 10.99573437649350538, 9.772747244158498603, 38.14042781937034476 ) ) ;
#515 = CARTESIAN_POINT ( 'NONE',  ( 4.709709529607406964, -13.90855959397108954, 38.16103891068024012 ) ) ;
#516 = ORIENTED_EDGE ( 'NONE', *, *, #2045, .F. ) ;
#517 = DIRECTION ( 'NONE',  ( 0.5000000000000099920, -0.8660254037844329345, 0.000000000000000000 ) ) ;
#518 = LINE ( 'NONE', #4350, #5754 ) ;
#519 = FACE_OUTER_BOUND ( 'NONE', #1704, .T. ) ;
#520 = ORIENTED_EDGE ( 'NONE', *, *, #3591, .F. ) ;
#521 = EDGE_CURVE ( 'NONE', #4734, #5727, #5427, .T. ) ;
#522 = DIRECTION ( 'NONE',  ( -1.000000000000000000, 0.000000000000000000, 0.000000000000000000 ) ) ;
#523 = CARTESIAN_POINT ( 'NONE',  ( 9.245260337044127752, -9.269614772507658529, 25.40693856330804934 ) ) ;
#524 = ORIENTED_EDGE ( 'NONE', *, *, #5142, .T. ) ;
#525 = EDGE_LOOP ( 'NONE', ( #4665, #4401 ) ) ;
#526 = CARTESIAN_POINT ( 'NONE',  ( -9.999999999999998224, -9.999999999999998224, 23.00000000000000000 ) ) ;
#527 = CARTESIAN_POINT ( 'NONE',  ( 15.00000000000000000, 50.91502622129181788, -35.00000000000000000 ) ) ;
#528 = FACE_OUTER_BOUND ( 'NONE', #1887, .T. ) ;
#529 = CARTESIAN_POINT ( 'NONE',  ( 0.000000000000000000, 0.000000000000000000, 0.000000000000000000 ) ) ;
#530 = DIRECTION ( 'NONE',  ( 0.3607836771741718129, -0.9326495259660421144, 0.000000000000000000 ) ) ;
#531 = EDGE_CURVE ( 'NONE', #5256, #4984, #2504, .T. ) ;
#532 = CARTESIAN_POINT ( 'NONE',  ( 9.933255351449995274, -9.419333092093014059, 30.50691708577705796 ) ) ;
#533 = ORIENTED_EDGE ( 'NONE', *, *, #4248, .T. ) ;
#534 = CARTESIAN_POINT ( 'NONE',  ( 6.095889600840177280, 10.32655419438761690, 28.09296952102860701 ) ) ;
#535 = CARTESIAN_POINT ( 'NONE',  ( 6.642184745761470666, 9.939337621248920840, 22.73823205004162418 ) ) ;
#536 = DIRECTION ( 'NONE',  ( 1.000000000000000000, 0.000000000000000000, 0.000000000000000000 ) ) ;
#537 = VERTEX_POINT ( 'NONE', #4039 ) ;
#538 = LINE ( 'NONE', #2882, #759 ) ;
#539 = CARTESIAN_POINT ( 'NONE',  ( -10.38144361273100635, -10.38144361273100458, 38.10175261887127363 ) ) ;
#540 = CARTESIAN_POINT ( 'NONE',  ( 0.000000000000000000, 67.50000000000000000, 20.00000000000000000 ) ) ;
#541 = DIRECTION ( 'NONE',  ( -0.000000000000000000, -0.000000000000000000, -1.000000000000000000 ) ) ;
#542 = CARTESIAN_POINT ( 'NONE',  ( 9.676903716103607778, -11.04476983075560348, 38.07288907902118069 ) ) ;
#543 = ORIENTED_EDGE ( 'NONE', *, *, #2903, .T. ) ;
#544 = CARTESIAN_POINT ( 'NONE',  ( 30.10043906316099083, 27.60043906316109386, -35.00000000000000000 ) ) ;
#545 = CARTESIAN_POINT ( 'NONE',  ( -57.58482424179695869, -72.37680137756228760, 40.00000000000000000 ) ) ;
#546 = ORIENTED_EDGE ( 'NONE', *, *, #4887, .T. ) ;
#547 = CARTESIAN_POINT ( 'NONE',  ( 12.71058384521441198, -7.353037798771444145, 38.12486502407008970 ) ) ;
#548 = CARTESIAN_POINT ( 'NONE',  ( 4.954970571217797826, -13.90079966151758306, 38.30990426830500439 ) ) ;
#549 = ORIENTED_EDGE ( 'NONE', *, *, #553, .F. ) ;
#550 =( NAMED_UNIT ( * ) PLANE_ANGLE_UNIT ( ) SI_UNIT ( $, .RADIAN. ) );
#551 = EDGE_LOOP ( 'NONE', ( #5803, #2026, #2863, #2751, #5984, #4013, #6009 ) ) ;
#552 = DIRECTION ( 'NONE',  ( 1.000000000000000000, 0.000000000000000000, 0.000000000000000000 ) ) ;
#553 = EDGE_CURVE ( 'NONE', #1998, #3523, #5960, .T. ) ;
#554 = DIRECTION ( 'NONE',  ( 0.9326495259660492199, -0.3607836771741531612, 0.000000000000000000 ) ) ;
#555 = CARTESIAN_POINT ( 'NONE',  ( 25.10043906316099083, 27.60043906316109386, 35.00000000000000000 ) ) ;
#556 = DIRECTION ( 'NONE',  ( 1.000000000000000000, 0.000000000000000000, 0.000000000000000000 ) ) ;
#557 = DIRECTION ( 'NONE',  ( -1.000000000000000000, 0.000000000000000000, 0.000000000000000000 ) ) ;
#558 = CARTESIAN_POINT ( 'NONE',  ( -9.192833548570215285, -59.02994620157096506, -35.00000000000000000 ) ) ;
#559 = VERTEX_POINT ( 'NONE', #5493 ) ;
#560 = ORIENTED_EDGE ( 'NONE', *, *, #3380, .F. ) ;
#561 = EDGE_CURVE ( 'NONE', #4523, #1252, #2256, .T. ) ;
#562 = CARTESIAN_POINT ( 'NONE',  ( -0.9833031778629136577, 13.77854189090673742, 35.81030296219172726 ) ) ;
#563 = B_SPLINE_CURVE_WITH_KNOTS ( 'NONE', 3,
 ( #1838, #2310, #4749, #406 ),
 .UNSPECIFIED., .F., .F.,
 ( 4, 4 ),
 ( 0.000000000000000000, 0.001907370850883698165 ),
 .UNSPECIFIED. ) ;
#564 = LINE ( 'NONE', #600, #3153 ) ;
#565 = DIRECTION ( 'NONE',  ( 0.5000000000000099920, -0.8660254037844328234, 0.000000000000000000 ) ) ;
#566 = AXIS2_PLACEMENT_3D ( 'NONE', #3993, #150, #2542 ) ;
#567 = ORIENTED_EDGE ( 'NONE', *, *, #2161, .F. ) ;
#568 = CARTESIAN_POINT ( 'NONE',  ( -0.000000000000000000, 50.91502622129181788, -35.00000000000000000 ) ) ;
#569 = CARTESIAN_POINT ( 'NONE',  ( -11.71459457793454995, -6.400384853991337941, 33.18278774224378225 ) ) ;
#570 = VECTOR ( 'NONE', #4474, 1000.000000000000114 ) ;
#571 = CIRCLE ( 'NONE', #574, 5.000000000000004441 ) ;
#572 = CARTESIAN_POINT ( 'NONE',  ( -9.166666666666673180, -9.999999999999998224, 23.00000000000000000 ) ) ;
#573 = VECTOR ( 'NONE', #1210, 1000.000000000000000 ) ;
#574 = AXIS2_PLACEMENT_3D ( 'NONE', #4413, #3909, #5042 ) ;
#575 = DIRECTION ( 'NONE',  ( 1.000000000000000000, 0.000000000000000000, 0.000000000000000000 ) ) ;
#576 = DIRECTION ( 'NONE',  ( -0.000000000000000000, -0.000000000000000000, -1.000000000000000000 ) ) ;
#577 = AXIS2_PLACEMENT_3D ( 'NONE', #2190, #3584, #5527 ) ;
#578 = ORIENTED_EDGE ( 'NONE', *, *, #154, .F. ) ;
#579 = PLANE ( 'NONE',  #2348 ) ;
#580 = CARTESIAN_POINT ( 'NONE',  ( 54.99999999999975131, 21.27605460800048576, 35.00000000000000000 ) ) ;
#581 = AXIS2_PLACEMENT_3D ( 'NONE', #4822, #2458, #104 ) ;
#582 = EDGE_CURVE ( 'NONE', #3886, #1816, #1139, .T. ) ;
#583 = ORIENTED_EDGE ( 'NONE', *, *, #2978, .F. ) ;
#584 = CARTESIAN_POINT ( 'NONE',  ( 0.000000000000000000, 0.000000000000000000, 20.00000000000000000 ) ) ;
#585 = DIRECTION ( 'NONE',  ( 0.000000000000000000, 0.000000000000000000, 1.000000000000000000 ) ) ;
#586 = CARTESIAN_POINT ( 'NONE',  ( 7.077301327650767249, -10.77711034800893231, 30.61076202992614625 ) ) ;
#587 = VECTOR ( 'NONE', #3050, 1000.000000000000000 ) ;
#588 = ORIENTED_EDGE ( 'NONE', *, *, #1150, .T. ) ;
#589 = CARTESIAN_POINT ( 'NONE',  ( 0.000000000000000000, 0.000000000000000000, -39.00000000000002842 ) ) ;
#590 = ORIENTED_EDGE ( 'NONE', *, *, #2017, .F. ) ;
#591 = FACE_OUTER_BOUND ( 'NONE', #2563, .T. ) ;
#592 = CARTESIAN_POINT ( 'NONE',  ( 9.074396217167167933, 58.26942451214404173, -35.00000000000000000 ) ) ;
#593 = DIRECTION ( 'NONE',  ( 1.000000000000000000, 0.000000000000000000, 0.000000000000000000 ) ) ;
#594 = DIRECTION ( 'NONE',  ( 0.000000000000000000, 0.000000000000000000, 1.000000000000000000 ) ) ;
#595 = CARTESIAN_POINT ( 'NONE',  ( 10.50531938289192624, -7.869812776064898152, 30.57803900350706527 ) ) ;
#596 = EDGE_CURVE ( 'NONE', #2998, #2186, #5952, .T. ) ;
#597 = ORIENTED_EDGE ( 'NONE', *, *, #5990, .T. ) ;
#598 = AXIS2_PLACEMENT_3D ( 'NONE', #1255, #5092, #897 ) ;
#599 = CARTESIAN_POINT ( 'NONE',  ( 3.531766105781286580, 10.70751178813581461, 28.15279191876807374 ) ) ;
#600 = CARTESIAN_POINT ( 'NONE',  ( -57.58482424179535997, 72.37680137756343868, -79.99999999999998579 ) ) ;
#601 = DIRECTION ( 'NONE',  ( 1.000000000000000000, 0.000000000000000000, 0.000000000000000000 ) ) ;
#602 = ORIENTED_EDGE ( 'NONE', *, *, #777, .T. ) ;
#603 = CARTESIAN_POINT ( 'NONE',  ( 27.50000000000000355, 47.63139720814412215, 35.00000000000000000 ) ) ;
#604 = AXIS2_PLACEMENT_3D ( 'NONE', #3810, #5171, #2796 ) ;
#605 = EDGE_CURVE ( 'NONE', #2868, #2500, #2363, .T. ) ;
#606 = CARTESIAN_POINT ( 'NONE',  ( -10.59948853791303414, -4.399300199984967463, 28.13666499103235452 ) ) ;
#607 = VECTOR ( 'NONE', #1106, 1000.000000000000000 ) ;
#608 = ORIENTED_EDGE ( 'NONE', *, *, #1198, .T. ) ;
#609 = TOROIDAL_SURFACE ( 'NONE', #5864, 5.141101056459331353, 10.00000000000000000 ) ;
#610 = CARTESIAN_POINT ( 'NONE',  ( -8.333333333333348136, -9.999999999999998224, 23.00000000000000000 ) ) ;
#611 = AXIS2_PLACEMENT_3D ( 'NONE', #84, #455, #3766 ) ;
#612 = ADVANCED_FACE ( 'NONE', ( #1767 ), #4186, .F. ) ;
#613 = CARTESIAN_POINT ( 'NONE',  ( 10.12138240269938905, 10.27356722921338950, 35.55812462721154787 ) ) ;
#614 = DIRECTION ( 'NONE',  ( 1.000000000000000000, 0.000000000000000000, 0.000000000000000000 ) ) ;
#615 = CIRCLE ( 'NONE', #5164, 15.67638808697555142 ) ;
#616 = ORIENTED_EDGE ( 'NONE', *, *, #432, .F. ) ;
#617 = CARTESIAN_POINT ( 'NONE',  ( -56.10121673609948090, 46.04269404270066701, 35.00000000000000000 ) ) ;
#618 = DIRECTION ( 'NONE',  ( 1.000000000000000000, 0.000000000000000000, 0.000000000000000000 ) ) ;
#619 = CARTESIAN_POINT ( 'NONE',  ( 8.999999999999994671, -3.000437278975552235, 23.18288419282212587 ) ) ;
#620 = ORIENTED_EDGE ( 'NONE', *, *, #2697, .F. ) ;
#621 = CARTESIAN_POINT ( 'NONE',  ( 5.247549479766027147, -10.46302782743270754, 28.11481907968152427 ) ) ;
#622 = ORIENTED_EDGE ( 'NONE', *, *, #582, .T. ) ;
#623 = CARTESIAN_POINT ( 'NONE',  ( -74.61196207728391983, 28.86269417393235415, -35.00000000000000000 ) ) ;
#624 = ORIENTED_EDGE ( 'NONE', *, *, #3473, .T. ) ;
#625 = FACE_OUTER_BOUND ( 'NONE', #3417, .T. ) ;
#626 = DIRECTION ( 'NONE',  ( 0.000000000000000000, 0.000000000000000000, 1.000000000000000000 ) ) ;
#627 = DIRECTION ( 'NONE',  ( 1.000000000000000000, -5.551115123125782086E-17, 1.083109739416814174E-19 ) ) ;
#628 = CARTESIAN_POINT ( 'NONE',  ( -10.19629538388490353, -10.19629538392591428, 35.54424335298404714 ) ) ;
#629 = DIRECTION ( 'NONE',  ( 0.5000000000000103251, -0.8660254037844326014, 0.000000000000000000 ) ) ;
#630 = ORIENTED_EDGE ( 'NONE', *, *, #2851, .T. ) ;
#631 = ORIENTED_EDGE ( 'NONE', *, *, #1846, .F. ) ;
#632 = CARTESIAN_POINT ( 'NONE',  ( 0.8880320553140821360, 10.89081796499577059, 28.17941898721253580 ) ) ;
#633 = CARTESIAN_POINT ( 'NONE',  ( 7.178663235509286977, 13.97471987708211394, 38.00000000000000000 ) ) ;
#634 = CARTESIAN_POINT ( 'NONE',  ( -56.72666074499684896, -46.14586675604289212, 35.04915833130718994 ) ) ;
#635 = EDGE_CURVE ( 'NONE', #3286, #4672, #1728, .T. ) ;
#636 = ORIENTED_EDGE ( 'NONE', *, *, #827, .T. ) ;
#637 = FACE_OUTER_BOUND ( 'NONE', #3669, .T. ) ;
#638 = CARTESIAN_POINT ( 'NONE',  ( -13.68733454931619953, 1.968046268140568156, 35.80501179064255268 ) ) ;
#639 = ORIENTED_EDGE ( 'NONE', *, *, #959, .F. ) ;
#640 = CARTESIAN_POINT ( 'NONE',  ( 3.317157231508561122, -9.910574073276151807, 22.73823205004162773 ) ) ;
#641 = EDGE_CURVE ( 'NONE', #3470, #836, #1329, .T. ) ;
#642 = CARTESIAN_POINT ( 'NONE',  ( 12.45812449473958949, 3.759289558891020455, 33.24069098933200905 ) ) ;
#643 = CARTESIAN_POINT ( 'NONE',  ( 0.000000000000000000, 67.50000000000000000, 20.00000000000000000 ) ) ;
#644 = ORIENTED_EDGE ( 'NONE', *, *, #1662, .F. ) ;
#645 = CARTESIAN_POINT ( 'NONE',  ( -1.630640067418198669E-13, 67.50000000000002842, 35.00000000000000000 ) ) ;
#646 = EDGE_CURVE ( 'NONE', #1950, #464, #2666, .T. ) ;
#647 = CARTESIAN_POINT ( 'NONE',  ( 2.742560498089724241, -11.69030472852370828, 30.70728637550628903 ) ) ;
#648 = ORIENTED_EDGE ( 'NONE', *, *, #4917, .T. ) ;
#649 = SURFACE_STYLE_USAGE ( .BOTH. , #2897 ) ;
#650 = ORIENTED_EDGE ( 'NONE', *, *, #4683, .F. ) ;
#651 = DIRECTION ( 'NONE',  ( -0.000000000000000000, -0.000000000000000000, 1.000000000000000000 ) ) ;
#652 = PLANE ( 'NONE',  #5646 ) ;
#653 = CONTEXT_DEPENDENT_SHAPE_REPRESENTATION ( #3969, #5174 ) ;
#654 = CARTESIAN_POINT ( 'NONE',  ( 0.000000000000000000, 0.000000000000000000, 38.00000000000000000 ) ) ;
#655 = CYLINDRICAL_SURFACE ( 'NONE', #3963, 5.000000000000004441 ) ;
#656 = VERTEX_POINT ( 'NONE', #417 ) ;
#657 = ORIENTED_EDGE ( 'NONE', *, *, #2551, .F. ) ;
#658 = LINE ( 'NONE', #396, #3915 ) ;
#659 = DIRECTION ( 'NONE',  ( 1.000000000000000000, 0.000000000000000000, 0.000000000000000000 ) ) ;
#660 = DIRECTION ( 'NONE',  ( -0.5000000000000019984, 0.8660254037844375974, 0.000000000000000000 ) ) ;
#661 = EDGE_LOOP ( 'NONE', ( #1061, #4979, #2915, #140, #3754, #1581, #2888, #2462, #2821, #639, #1009, #3061, #3078, #887, #3758, #1992 ) ) ;
#662 = DIRECTION ( 'NONE',  ( 0.1538769332794358846, 0.9880900209011910240, 0.000000000000000000 ) ) ;
#663 = CARTESIAN_POINT ( 'NONE',  ( -12.60026679007840933, -2.830884587392748397, 33.25110354061415308 ) ) ;
#664 = ORIENTED_EDGE ( 'NONE', *, *, #2969, .F. ) ;
#665 = CARTESIAN_POINT ( 'NONE',  ( 1.082228759108211813, -15.67638808697554786, 38.00000000000000711 ) ) ;
#666 = CIRCLE ( 'NONE', #1719, 5.000000000000004441 ) ;
#667 = ADVANCED_FACE ( 'NONE', ( #3633 ), #5550, .T. ) ;
#668 = EDGE_CURVE ( 'NONE', #5813, #4909, #2649, .T. ) ;
#669 = CARTESIAN_POINT ( 'NONE',  ( 12.74240908541723805, 1.902479615894477449, 33.26151609189631841 ) ) ;
#670 = VERTEX_POINT ( 'NONE', #3233 ) ;
#671 = CARTESIAN_POINT ( 'NONE',  ( 8.999999999988068211, 9.000000000000005329, 23.06137295785747554 ) ) ;
#672 = AXIS2_PLACEMENT_3D ( 'NONE', #3089, #1561, #4041 ) ;
#673 = SURFACE_STYLE_FILL_AREA ( #4058 ) ;
#674 = CARTESIAN_POINT ( 'NONE',  ( 0.000000000000000000, 0.000000000000000000, 40.00000000000000000 ) ) ;
#675 = EDGE_CURVE ( 'NONE', #4909, #1654, #1700, .T. ) ;
#676 = CARTESIAN_POINT ( 'NONE',  ( -4.273055220303960233, -9.778265677387510735, 25.59105958838677708 ) ) ;
#677 = CIRCLE ( 'NONE', #4732, 5.000000000000005329 ) ;
#678 = EDGE_LOOP ( 'NONE', ( #3714, #1117 ) ) ;
#679 = CARTESIAN_POINT ( 'NONE',  ( 62.30180741492871022, 50.18450749816254586, 38.99999999999995737 ) ) ;
#680 = ORIENTED_EDGE ( 'NONE', *, *, #2232, .T. ) ;
#681 = CARTESIAN_POINT ( 'NONE',  ( 54.99999999999975131, 21.27605460800048576, -35.00000000000000000 ) ) ;
#682 = CIRCLE ( 'NONE', #778, 4.999999999999990230 ) ;
#683 = DIRECTION ( 'NONE',  ( 0.3607836771741718684, -0.9326495259660421144, 0.000000000000000000 ) ) ;
#684 =( GEOMETRIC_REPRESENTATION_CONTEXT ( 3 ) GLOBAL_UNCERTAINTY_ASSIGNED_CONTEXT ( ( #3684 ) ) GLOBAL_UNIT_ASSIGNED_CONTEXT ( ( #1802, #340, #1744 ) ) REPRESENTATION_CONTEXT ( 'NONE', 'WORKASPACE' ) );
#685 = FACE_OUTER_BOUND ( 'NONE', #2877, .T. ) ;
#686 = PLANE ( 'NONE',  #475 ) ;
#687 = VECTOR ( 'NONE', #1691, 1000.000000000000000 ) ;
#688 = VERTEX_POINT ( 'NONE', #2707 ) ;
#689 = CARTESIAN_POINT ( 'NONE',  ( 8.159736356077655017, 11.57174281757876955, 35.66679457777021156 ) ) ;
#690 = CARTESIAN_POINT ( 'NONE',  ( 13.47611570251764768, 8.069545871843432749, 37.99999999999999289 ) ) ;
#691 =( NAMED_UNIT ( * ) PLANE_ANGLE_UNIT ( ) SI_UNIT ( $, .RADIAN. ) );
#692 = ORIENTED_EDGE ( 'NONE', *, *, #2352, .F. ) ;
#693 = DIRECTION ( 'NONE',  ( 1.154631945610162802E-14, -1.000000000000000000, 0.000000000000000000 ) ) ;
#694 = CARTESIAN_POINT ( 'NONE',  ( -12.81596724893641337, 1.499651672263871603E-14, 33.26667497053200151 ) ) ;
#695 = APPLICATION_CONTEXT ( 'automotive_design' ) ;
#696 = ORIENTED_EDGE ( 'NONE', *, *, #3568, .F. ) ;
#697 = CARTESIAN_POINT ( 'NONE',  ( 57.58482424179591419, -72.37680137756305498, -79.99999999999998579 ) ) ;
#698 = EDGE_CURVE ( 'NONE', #2060, #2569, #1468, .T. ) ;
#699 = DIRECTION ( 'NONE',  ( 0.9326495259660493309, -0.3607836771741531612, 0.000000000000000000 ) ) ;
#700 = VECTOR ( 'NONE', #2496, 1000.000000000000000 ) ;
#701 = B_SPLINE_CURVE_WITH_KNOTS ( 'NONE', 3,
 ( #3878, #4820, #3382, #5294 ),
 .UNSPECIFIED., .F., .F.,
 ( 4, 4 ),
 ( 0.000000000000000000, 0.001907370850886569132 ),
 .UNSPECIFIED. ) ;
#702 = CARTESIAN_POINT ( 'NONE',  ( 9.708537589994000072, 5.113933401365464704, 25.56820946177495557 ) ) ;
#703 = CIRCLE ( 'NONE', #1276, 5.000000000000004441 ) ;
#704 = DIRECTION ( 'NONE',  ( 1.000000000000000000, 0.000000000000000000, 0.000000000000000000 ) ) ;
#705 = VERTEX_POINT ( 'NONE', #4161 ) ;
#706 = CARTESIAN_POINT ( 'NONE',  ( 0.000000000000000000, 12.00000000000000355, 35.00000000000000000 ) ) ;
#707 = VECTOR ( 'NONE', #2728, 1000.000000000000000 ) ;
#708 = EDGE_CURVE ( 'NONE', #2370, #5794, #356, .T. ) ;
#709 = DIRECTION ( 'NONE',  ( -0.8660254037844339337, -0.5000000000000079936, 0.000000000000000000 ) ) ;
#710 = AXIS2_PLACEMENT_3D ( 'NONE', #1909, #3290, #2419 ) ;
#711 = CARTESIAN_POINT ( 'NONE',  ( -1.117102909420315718E-14, -13.77854189090673742, 35.81030296219173437 ) ) ;
#712 = ORIENTED_EDGE ( 'NONE', *, *, #2311, .T. ) ;
#713 = ORIENTED_EDGE ( 'NONE', *, *, #1737, .T. ) ;
#714 = CARTESIAN_POINT ( 'NONE',  ( 14.58318388806640442, 1.909955344851026027, 38.18050947768620063 ) ) ;
#715 = DIRECTION ( 'NONE',  ( 0.000000000000000000, 0.000000000000000000, 1.000000000000000000 ) ) ;
#716 = ADVANCED_FACE ( 'NONE', ( #885 ), #3690, .T. ) ;
#717 = CARTESIAN_POINT ( 'NONE',  ( -10.00265588554885454, -10.00265588554885454, 33.03935750738951782 ) ) ;
#718 = DIRECTION ( 'NONE',  ( -1.000000000000000000, 0.000000000000000000, 0.000000000000000000 ) ) ;
#719 = VERTEX_POINT ( 'NONE', #6045 ) ;
#720 = VERTEX_POINT ( 'NONE', #3203 ) ;
#721 = CARTESIAN_POINT ( 'NONE',  ( 7.610208295502498999, 9.462636878983097688, 25.48187184588751464 ) ) ;
#722 = CARTESIAN_POINT ( 'NONE',  ( 0.000000000000000000, 0.000000000000000000, -39.00000000000001421 ) ) ;
#723 = EDGE_CURVE ( 'NONE', #2393, #4821, #2733, .T. ) ;
#724 = ORIENTED_EDGE ( 'NONE', *, *, #4597, .T. ) ;
#725 = CARTESIAN_POINT ( 'NONE',  ( -8.964120776013636771, -3.322926169935023655, 23.06129021161080317 ) ) ;
#726 = EDGE_LOOP ( 'NONE', ( #3570, #4220, #4699, #3819 ) ) ;
#727 = DIRECTION ( 'NONE',  ( 0.000000000000000000, 0.000000000000000000, 1.000000000000000000 ) ) ;
#728 = CARTESIAN_POINT ( 'NONE',  ( 13.50805179034378689, 5.845970755595363499, 38.28811402100272687 ) ) ;
#729 = CARTESIAN_POINT ( 'NONE',  ( 9.999999999999998224, 9.999999999999998224, 20.00000000000000000 ) ) ;
#730 = VERTEX_POINT ( 'NONE', #6073 ) ;
#731 = ORIENTED_EDGE ( 'NONE', *, *, #4522, .T. ) ;
#732 = CARTESIAN_POINT ( 'NONE',  ( 99.00000000000000000, 0.000000000000000000, -40.00000000000000000 ) ) ;
#733 = CARTESIAN_POINT ( 'NONE',  ( -4.807771419025854698, -13.07374771013670411, 35.76776546669864132 ) ) ;
#734 = ORIENTED_EDGE ( 'NONE', *, *, #4098, .T. ) ;
#735 = CARTESIAN_POINT ( 'NONE',  ( -8.999999999999994671, 3.000437278975516708, 23.18288419282211521 ) ) ;
#736 = EDGE_LOOP ( 'NONE', ( #1054, #1574, #5921, #216, #1999, #3686, #5636 ) ) ;
#737 = DIRECTION ( 'NONE',  ( -0.000000000000000000, -0.000000000000000000, -1.000000000000000000 ) ) ;
#738 = CARTESIAN_POINT ( 'NONE',  ( -58.45671475544979501, 33.74999999999974420, 35.00000000000000000 ) ) ;
#739 = ITEM_DEFINED_TRANSFORMATION ( 'NONE', 'NONE', #3144,  #73 ) ;
#740 = CARTESIAN_POINT ( 'NONE',  ( -57.35713647666923976, 46.20154318182412112, 35.13717928826270054 ) ) ;
#741 = CARTESIAN_POINT ( 'NONE',  ( -58.45671475544946816, -33.75000000000027711, -35.00000000000000000 ) ) ;
#742 = EDGE_CURVE ( 'NONE', #5503, #2020, #5457, .T. ) ;
#743 = EDGE_LOOP ( 'NONE', ( #123, #3043, #1631, #4334 ) ) ;
#744 = CARTESIAN_POINT ( 'NONE',  ( 9.632247231687292910, 10.63625351335941716, 35.59852902770369809 ) ) ;
#745 = CARTESIAN_POINT ( 'NONE',  ( 15.12434353048566571, -4.260267006495016773, 38.00000000000000711 ) ) ;
#746 = CARTESIAN_POINT ( 'NONE',  ( -15.67638808697555142, -2.609965535188016420E-15, 38.00000000000000711 ) ) ;
#747 = VERTEX_POINT ( 'NONE', #5634 ) ;
#748 = CARTESIAN_POINT ( 'NONE',  ( -62.30180741492891627, 50.18450749816232559, -35.00000000000000711 ) ) ;
#749 = EDGE_CURVE ( 'NONE', #2774, #3309, #93, .T. ) ;
#750 = CARTESIAN_POINT ( 'NONE',  ( -10.67320828294309898, 8.785766938566926143, 33.09220912812762094 ) ) ;
#751 = EDGE_LOOP ( 'NONE', ( #4191, #5188, #5078, #271 ) ) ;
#752 = CARTESIAN_POINT ( 'NONE',  ( -10.27356722921338950, 10.12138240269938905, 35.55812462721154787 ) ) ;
#753 = FACE_BOUND ( 'NONE', #1300, .T. ) ;
#754 = CARTESIAN_POINT ( 'NONE',  ( 10.23352841777492017, 8.662324224478986423, 30.54531597708798074 ) ) ;
#755 = CARTESIAN_POINT ( 'NONE',  ( 25.10043906316099083, 27.60043906316109386, -35.00000000000000000 ) ) ;
#756 = ORIENTED_EDGE ( 'NONE', *, *, #2983, .F. ) ;
#757 = EDGE_LOOP ( 'NONE', ( #1083, #1609, #1805, #974, #3958 ) ) ;
#758 = B_SPLINE_CURVE_WITH_KNOTS ( 'NONE', 3,
 ( #38, #2893, #943, #4797, #547, #2366, #1364, #5699, #2425, #1916, #4261, #3269, #2864, #4768 ),
 .UNSPECIFIED., .F., .F.,
 ( 4, 2, 2, 2, 2, 2, 4 ),
 ( 2.453269466693398698E-18, 0.002860246893306488992, 0.004290370339959730453, 0.005720493786612971913, 0.008580740679919452232, 0.01001086412657269456, 0.01144098757322593515 ),
 .UNSPECIFIED. ) ;
#759 = VECTOR ( 'NONE', #5814, 1000.000000000000114 ) ;
#760 = CARTESIAN_POINT ( 'NONE',  ( -3.759380242563084451, -12.45811160333930800, 33.24069127598783524 ) ) ;
#761 = ORIENTED_EDGE ( 'NONE', *, *, #4032, .F. ) ;
#762 = DIRECTION ( 'NONE',  ( 1.000000000000000000, 0.000000000000000000, 0.000000000000000000 ) ) ;
#763 = AXIS2_PLACEMENT_3D ( 'NONE', #4089, #6004, #1717 ) ;
#764 = VERTEX_POINT ( 'NONE', #767 ) ;
#765 = CARTESIAN_POINT ( 'NONE',  ( 7.182140071210238271E-14, -8.916303653273167033E-14, -35.00000000000000000 ) ) ;
#766 = VECTOR ( 'NONE', #3692, 1000.000000000000000 ) ;
#767 = CARTESIAN_POINT ( 'NONE',  ( -11.50000000000000355, 67.50000000000000000, 20.00000000000000000 ) ) ;
#768 = PRODUCT_CONTEXT ( 'NONE', #487, 'mechanical' ) ;
#769 = DIRECTION ( 'NONE',  ( 0.000000000000000000, 0.000000000000000000, 1.000000000000000000 ) ) ;
#770 = CARTESIAN_POINT ( 'NONE',  ( -9.969668718019493170, -9.144590365090015993, 22.73823205004162418 ) ) ;
#771 = ORIENTED_EDGE ( 'NONE', *, *, #5079, .T. ) ;
#772 = DIRECTION ( 'NONE',  ( -0.000000000000000000, 0.000000000000000000, 1.000000000000000000 ) ) ;
#773 = LINE ( 'NONE', #3989, #1060 ) ;
#774 = CARTESIAN_POINT ( 'NONE',  ( 14.79903580929011753, 5.273949241992679227, 38.00000000000000711 ) ) ;
#776 = AXIS2_PLACEMENT_3D ( 'NONE', #4465, #4518, #311 ) ;
#775 = DIRECTION ( 'NONE',  ( -0.7787725926866081450, -0.6273063437270328668, 0.000000000000000000 ) ) ;
#777 = EDGE_CURVE ( 'NONE', #5916, #5503, #4544, .T. ) ;
#778 = AXIS2_PLACEMENT_3D ( 'NONE', #3943, #2076, #5392 ) ;
#779 = ADVANCED_FACE ( 'NONE', ( #5517 ), #330, .T. ) ;
#780 = ORIENTED_EDGE ( 'NONE', *, *, #3835, .F. ) ;
#781 = DIRECTION ( 'NONE',  ( -0.000000000000000000, 0.000000000000000000, 1.000000000000000000 ) ) ;
#782 = AXIS2_PLACEMENT_3D ( 'NONE', #81, #1086, #4804 ) ;
#783 = CARTESIAN_POINT ( 'NONE',  ( -10.99573437649350183, 9.772747244158500379, 38.14042781937034476 ) ) ;
#784 = ORIENTED_EDGE ( 'NONE', *, *, #438, .F. ) ;
#785 = CARTESIAN_POINT ( 'NONE',  ( -9.772747244158496827, 10.99573437649350538, 38.14042781937034476 ) ) ;
#786 = CARTESIAN_POINT ( 'NONE',  ( 0.000000000000000000, 0.000000000000000000, -39.00000000000002842 ) ) ;
#787 = EDGE_CURVE ( 'NONE', #2393, #1473, #5668, .T. ) ;
#788 = AXIS2_PLACEMENT_3D ( 'NONE', #722, #4046, #659 ) ;
#789 = PLANE ( 'NONE',  #3246 ) ;
#790 = AXIS2_PLACEMENT_3D ( 'NONE', #1923, #3303, #593 ) ;
#791 = CARTESIAN_POINT ( 'NONE',  ( -4.130675435985315210E-14, -1.067806758184287486E-13, 35.00000000000000000 ) ) ;
#792 = ORIENTED_EDGE ( 'NONE', *, *, #641, .F. ) ;
#793 = EDGE_CURVE ( 'NONE', #354, #5786, #5696, .T. ) ;
#794 = AXIS2_PLACEMENT_3D ( 'NONE', #2565, #4454, #4637 ) ;
#795 = CARTESIAN_POINT ( 'NONE',  ( -7.228600378928581982, -11.39263409468387422, 33.15620577507543487 ) ) ;
#796 = ORIENTED_EDGE ( 'NONE', *, *, #3047, .T. ) ;
#797 = CARTESIAN_POINT ( 'NONE',  ( 67.92475106770271509, 25.56373185532915926, 35.00000000000000000 ) ) ;
#798 = CIRCLE ( 'NONE', #5654, 4.999999999999997335 ) ;
#799 = ORIENTED_EDGE ( 'NONE', *, *, #787, .F. ) ;
#800 = DIRECTION ( 'NONE',  ( 1.000000000000000000, 0.000000000000000000, 0.000000000000000000 ) ) ;
#801 = CARTESIAN_POINT ( 'NONE',  ( 0.000000000000000000, 0.000000000000000000, 38.00000000000000000 ) ) ;
#802 = CIRCLE ( 'NONE', #3651, 5.000000000000004441 ) ;
#803 =( GEOMETRIC_REPRESENTATION_CONTEXT ( 3 ) GLOBAL_UNCERTAINTY_ASSIGNED_CONTEXT ( ( #3805 ) ) GLOBAL_UNIT_ASSIGNED_CONTEXT ( ( #5845, #5678, #19 ) ) REPRESENTATION_CONTEXT ( 'NONE', 'WORKASPACE' ) );
#804 = DIRECTION ( 'NONE',  ( -0.7787725926866118087, 0.6273063437270282039, 0.000000000000000000 ) ) ;
#805 = CARTESIAN_POINT ( 'NONE',  ( -9.999999999999998224, 3.333333333333377890, 23.00000000000000000 ) ) ;
#806 = AXIS2_PLACEMENT_3D ( 'NONE', #2341, #23, #1529 ) ;
#807 = DIRECTION ( 'NONE',  ( -0.7787725926866080339, -0.6273063437270329779, 0.000000000000000000 ) ) ;
#808 = ORIENTED_EDGE ( 'NONE', *, *, #6021, .T. ) ;
#809 = DIRECTION ( 'NONE',  ( -0.000000000000000000, -0.000000000000000000, -1.000000000000000000 ) ) ;
#810 = DIRECTION ( 'NONE',  ( 0.7071067811865489050, 0.000000000000000000, 0.7071067811865462405 ) ) ;
#811 = FILL_AREA_STYLE ('',( #5061 ) ) ;
#812 =( NAMED_UNIT ( * ) SI_UNIT ( $, .STERADIAN. ) SOLID_ANGLE_UNIT ( ) );
#813 =( REPRESENTATION_RELATIONSHIP ('NONE','NONE', #4716, #4975 ) REPRESENTATION_RELATIONSHIP_WITH_TRANSFORMATION ( #1197 )SHAPE_REPRESENTATION_RELATIONSHIP( ) );
#814 = CARTESIAN_POINT ( 'NONE',  ( 13.77854189090674097, -0.9833031778629309771, 35.81030296219172726 ) ) ;
#815 = CARTESIAN_POINT ( 'NONE',  ( -11.03292118881348394, 8.007183658747754507, 33.12420745160153501 ) ) ;
#816 = VERTEX_POINT ( 'NONE', #3780 ) ;
#817 = CARTESIAN_POINT ( 'NONE',  ( -6.248091806769195955, 11.02058084744346189, 30.63788045528724524 ) ) ;
#818 = EDGE_CURVE ( 'NONE', #4790, #2604, #4823, .T. ) ;
#819 = DIRECTION ( 'NONE',  ( -0.7071067811865474617, 8.659560562354932858E-17, 0.7071067811865474617 ) ) ;
#820 = CARTESIAN_POINT ( 'NONE',  ( 8.999999999999994671, 6.000509662810391553, 23.13502399099459339 ) ) ;
#821 = DIRECTION ( 'NONE',  ( 1.000000000000000000, -5.329070518200750605E-15, 0.000000000000000000 ) ) ;
#822 = EDGE_CURVE ( 'NONE', #5813, #2500, #2325, .T. ) ;
#823 = DIRECTION ( 'NONE',  ( -0.7787725926866162496, 0.6273063437270229858, 0.000000000000000000 ) ) ;
#824 = EDGE_LOOP ( 'NONE', ( #1358, #407, #4198, #2211 ) ) ;
#825 = PRODUCT ( 'MAS-319', 'MAS-319', '', ( #5020 ) ) ;
#826 = CARTESIAN_POINT ( 'NONE',  ( -7.487361748921665061, -8.967351122863068014, 22.92808036848186859 ) ) ;
#827 = EDGE_CURVE ( 'NONE', #4272, #1861, #444, .T. ) ;
#828 = ORIENTED_EDGE ( 'NONE', *, *, #4445, .T. ) ;
#829 = PLANE ( 'NONE',  #4757 ) ;
#830 = ORIENTED_EDGE ( 'NONE', *, *, #3407, .F. ) ;
#831 = DIRECTION ( 'NONE',  ( -0.000000000000000000, 0.000000000000000000, 1.000000000000000000 ) ) ;
#832 = DIRECTION ( 'NONE',  ( -0.000000000000000000, -0.000000000000000000, -1.000000000000000000 ) ) ;
#833 = CARTESIAN_POINT ( 'NONE',  ( 27.50000000000043698, -47.63139720814386635, 35.00000000000000000 ) ) ;
#834 = CARTESIAN_POINT ( 'NONE',  ( -9.999999999999998224, 5.833333333333365012, 23.00000000000000000 ) ) ;
#835 = DIRECTION ( 'NONE',  ( 1.000000000000000000, 0.000000000000000000, 0.000000000000000000 ) ) ;
#836 = VERTEX_POINT ( 'NONE', #2889 ) ;
#837 = CARTESIAN_POINT ( 'NONE',  ( 0.000000000000000000, 0.000000000000000000, 38.99999999999995737 ) ) ;
#838 = DIRECTION ( 'NONE',  ( -0.000000000000000000, -0.000000000000000000, -1.000000000000000000 ) ) ;
#839 = CARTESIAN_POINT ( 'NONE',  ( -6.488003555186317328, 13.19914683770227093, 38.13881399654477633 ) ) ;
#840 = CARTESIAN_POINT ( 'NONE',  ( 10.85317354580219629, -1.776706711792237492, 28.17414650202875137 ) ) ;
#841 = CARTESIAN_POINT ( 'NONE',  ( -8.963498645742985715, 4.986905650496099796, 23.01829711214647745 ) ) ;
#842 = ORIENTED_EDGE ( 'NONE', *, *, #5142, .F. ) ;
#843 = CARTESIAN_POINT ( 'NONE',  ( -5.390571672161838634, 11.22195964661421819, 30.65936073406735574 ) ) ;
#844 = CARTESIAN_POINT ( 'NONE',  ( 47.58482424179590708, -72.37680137756305498, 40.00000000000000000 ) ) ;
#845 = CARTESIAN_POINT ( 'NONE',  ( 74.61196207728340823, 28.86269417393367220, -35.00000000000000711 ) ) ;
#846 = CARTESIAN_POINT ( 'NONE',  ( -14.65251043020005461, 0.9663357036150521662, 38.18273246053422554 ) ) ;
#847 = UNCERTAINTY_MEASURE_WITH_UNIT (LENGTH_MEASURE( 1.000000000000000082E-05 ), #5340, 'distance_accuracy_value', 'NONE');
#848 = EDGE_CURVE ( 'NONE', #3788, #2202, #518, .T. ) ;
#849 = ADVANCED_FACE ( 'NONE', ( #1423, #6132 ), #4314, .F. ) ;
#850 = CARTESIAN_POINT ( 'NONE',  ( 62.30180741492923602, -50.18450749816189216, 35.00000000000000000 ) ) ;
#851 = ORIENTED_EDGE ( 'NONE', *, *, #3535, .F. ) ;
#852 = LINE ( 'NONE', #911, #5350 ) ;
#853 = ORIENTED_EDGE ( 'NONE', *, *, #513, .T. ) ;
#854 = CARTESIAN_POINT ( 'NONE',  ( 80.99999999999998579, 9.919639073093559622E-15, -40.00000000000000000 ) ) ;
#855 = DIRECTION ( 'NONE',  ( 1.000000000000000000, 0.000000000000000000, 0.000000000000000000 ) ) ;
#856 = EDGE_CURVE ( 'NONE', #1594, #1863, #4862, .T. ) ;
#857 = CARTESIAN_POINT ( 'NONE',  ( -15.12434353048566216, -4.260267006495012332, 37.99999999999999289 ) ) ;
#858 = DIRECTION ( 'NONE',  ( -0.000000000000000000, -0.000000000000000000, -1.000000000000000000 ) ) ;
#859 = CIRCLE ( 'NONE', #2034, 11.50000000000000178 ) ;
#860 = AXIS2_PLACEMENT_3D ( 'NONE', #418, #2296, #5237 ) ;
#861 = ORIENTED_EDGE ( 'NONE', *, *, #2673, .F. ) ;
#862 = DIRECTION ( 'NONE',  ( 1.000000000000000000, 0.000000000000000000, 0.000000000000000000 ) ) ;
#863 = CARTESIAN_POINT ( 'NONE',  ( -11.08488032081242558, -11.08488032081241847, 38.00000000000000000 ) ) ;
#864 = CARTESIAN_POINT ( 'NONE',  ( 1.937269431830858979, 14.55597330376932774, 38.18000980160653768 ) ) ;
#865 = CARTESIAN_POINT ( 'NONE',  ( 13.07374771013670589, -4.807771419025858251, 35.76776546669863421 ) ) ;
#866 = VECTOR ( 'NONE', #2323, 1000.000000000000000 ) ;
#867 = CARTESIAN_POINT ( 'NONE',  ( -12.24723121994939135, 4.666652649023722788, 33.22501677959694177 ) ) ;
#868 = CIRCLE ( 'NONE', #4025, 80.00000000000000000 ) ;
#869 = ORIENTED_EDGE ( 'NONE', *, *, #1198, .F. ) ;
#870 = VECTOR ( 'NONE', #3518, 1000.000000000000000 ) ;
#871 = CARTESIAN_POINT ( 'NONE',  ( -7.869812776064877724, 10.50531938289192624, 30.57803900350706172 ) ) ;
#872 = CARTESIAN_POINT ( 'NONE',  ( -81.00000000000004263, 9.919639073093567511E-15, 40.00000000000000000 ) ) ;
#873 = ORIENTED_EDGE ( 'NONE', *, *, #708, .T. ) ;
#874 = FACE_OUTER_BOUND ( 'NONE', #751, .T. ) ;
#875 =( GEOMETRIC_REPRESENTATION_CONTEXT ( 3 ) GLOBAL_UNCERTAINTY_ASSIGNED_CONTEXT ( ( #4308 ) ) GLOBAL_UNIT_ASSIGNED_CONTEXT ( ( #2245, #2215, #3729 ) ) REPRESENTATION_CONTEXT ( 'NONE', 'WORKASPACE' ) );
#876 = CIRCLE ( 'NONE', #5445, 5.000000000000004441 ) ;
#877 = DIRECTION ( 'NONE',  ( 1.000000000000000000, 0.000000000000000000, 0.000000000000000000 ) ) ;
#878 = DIRECTION ( 'NONE',  ( -1.000000000000000000, 0.000000000000000000, 0.000000000000000000 ) ) ;
#879 = CARTESIAN_POINT ( 'NONE',  ( -9.322893336083163618, -9.590870124851308631, 27.95908392747358917 ) ) ;
#880 = EDGE_LOOP ( 'NONE', ( #2654, #2905, #5186, #326 ) ) ;
#881 = CARTESIAN_POINT ( 'NONE',  ( -4.130675435985315210E-14, -1.067806758184287486E-13, 35.00000000000000000 ) ) ;
#882 = VERTEX_POINT ( 'NONE', #2422 ) ;
#883 = CARTESIAN_POINT ( 'NONE',  ( 85.08403291566575888, -27.64547812922912939, -40.00000000000000000 ) ) ;
#884 = ADVANCED_FACE ( 'NONE', ( #1985 ), #3751, .T. ) ;
#885 = FACE_OUTER_BOUND ( 'NONE', #1773, .T. ) ;
#886 = AXIS2_PLACEMENT_3D ( 'NONE', #105, #69, #3322 ) ;
#887 = ORIENTED_EDGE ( 'NONE', *, *, #2926, .F. ) ;
#888 = CARTESIAN_POINT ( 'NONE',  ( -12.35760627049922000, -9.696021465980068754, 37.99999999999998579 ) ) ;
#889 = AXIS2_PLACEMENT_3D ( 'NONE', #5137, #3747, #4633 ) ;
#890 = DIRECTION ( 'NONE',  ( 0.000000000000000000, 0.000000000000000000, -1.000000000000000000 ) ) ;
#891 = VECTOR ( 'NONE', #1166, 1000.000000000000000 ) ;
#892 = ORIENTED_EDGE ( 'NONE', *, *, #3835, .T. ) ;
#893 = VECTOR ( 'NONE', #5280, 999.9999999999998863 ) ;
#894 = DIRECTION ( 'NONE',  ( -0.000000000000000000, -0.000000000000000000, -1.000000000000000000 ) ) ;
#895 = EDGE_CURVE ( 'NONE', #2972, #5932, #3846, .T. ) ;
#896 = CARTESIAN_POINT ( 'NONE',  ( 50.91502622129181788, 15.00000000000000355, 35.00000000000000000 ) ) ;
#897 = DIRECTION ( 'NONE',  ( 1.000000000000000000, 0.000000000000000000, 0.000000000000000000 ) ) ;
#898 = SHAPE_REPRESENTATION_RELATIONSHIP ( 'NONE' , 'NONE' ,  #2176, #5744 ) ;
#899 = VECTOR ( 'NONE', #4486, 1000.000000000000000 ) ;
#900 = CARTESIAN_POINT ( 'NONE',  ( 9.778265677387498300, -4.273055220303958457, 25.59105958838677353 ) ) ;
#901 = CIRCLE ( 'NONE', #1670, 15.67638808697555142 ) ;
#902 = ORIENTED_EDGE ( 'NONE', *, *, #6125, .T. ) ;
#903 = ADVANCED_FACE ( 'NONE', ( #2395 ), #7, .F. ) ;
#904 = CARTESIAN_POINT ( 'NONE',  ( -8.432782529159778662, 9.370308598635419983, 25.44727941985334496 ) ) ;
#905 = CARTESIAN_POINT ( 'NONE',  ( 8.056095891487838412E-14, -1.254589464284425060E-14, 35.00000000000000000 ) ) ;
#906 = VERTEX_POINT ( 'NONE', #545 ) ;
#907 = DIRECTION ( 'NONE',  ( 1.000000000000000000, 0.000000000000000000, -0.000000000000000000 ) ) ;
#908 = CARTESIAN_POINT ( 'NONE',  ( -14.55721289103182237, 1.928061058260225558, 38.18004976450266952 ) ) ;
#909 = CARTESIAN_POINT ( 'NONE',  ( -9.086997423426605991, -11.58116666691846852, 38.17633527770230017 ) ) ;
#910 = EDGE_LOOP ( 'NONE', ( #49, #1213, #66, #5315 ) ) ;
#911 = CARTESIAN_POINT ( 'NONE',  ( 74.61196207728410457, -28.86269417393182479, 35.00000000000000000 ) ) ;
#912 = ORIENTED_EDGE ( 'NONE', *, *, #6122, .F. ) ;
#913 = DIRECTION ( 'NONE',  ( 1.000000000000000000, 1.154631945610162960E-14, -0.000000000000000000 ) ) ;
#914 = DIRECTION ( 'NONE',  ( -0.6273063437270228748, -0.7787725926866162496, 0.000000000000000000 ) ) ;
#915 = VERTEX_POINT ( 'NONE', #1011 ) ;
#916 = DIRECTION ( 'NONE',  ( -0.7787725926866118087, 0.6273063437270282039, 0.000000000000000000 ) ) ;
#917 = DIRECTION ( 'NONE',  ( -0.000000000000000000, -0.000000000000000000, -1.000000000000000000 ) ) ;
#918 = ORIENTED_EDGE ( 'NONE', *, *, #1893, .T. ) ;
#919 = ORIENTED_EDGE ( 'NONE', *, *, #5150, .F. ) ;
#920 = DIRECTION ( 'NONE',  ( -0.000000000000000000, -0.000000000000000000, -1.000000000000000000 ) ) ;
#921 = CARTESIAN_POINT ( 'NONE',  ( -57.58482424179535997, 72.37680137756343868, -40.00000000000000000 ) ) ;
#922 = DIRECTION ( 'NONE',  ( -1.000000000000000000, -8.673617379884027583E-15, 0.000000000000000000 ) ) ;
#923 =( LENGTH_UNIT ( ) NAMED_UNIT ( * ) SI_UNIT ( .MILLI., .METRE. ) );
#924 = CARTESIAN_POINT ( 'NONE',  ( 0.000000000000000000, 0.000000000000000000, 45.00000000000000711 ) ) ;
#925 = CARTESIAN_POINT ( 'NONE',  ( 11.22195964661421641, -5.390571672161878602, 30.65936073406735218 ) ) ;
#926 = ADVANCED_FACE ( 'NONE', ( #940 ), #2825, .F. ) ;
#927 = ORIENTED_EDGE ( 'NONE', *, *, #4966, .F. ) ;
#928 = CARTESIAN_POINT ( 'NONE',  ( -8.328520801854338629, 12.11088206474084750, 38.20782360758020957 ) ) ;
#929 = CARTESIAN_POINT ( 'NONE',  ( -11.08488032081242025, 11.08488032081242203, 38.00000000000000000 ) ) ;
#930 = LINE ( 'NONE', #958, #6029 ) ;
#931 = ORIENTED_EDGE ( 'NONE', *, *, #2696, .F. ) ;
#932 = DIRECTION ( 'NONE',  ( -0.000000000000000000, 0.000000000000000000, 1.000000000000000000 ) ) ;
#933 = ADVANCED_FACE ( 'NONE', ( #5767 ), #1912, .T. ) ;
#934 = DIRECTION ( 'NONE',  ( 0.000000000000000000, -1.000000000000000000, 0.000000000000000000 ) ) ;
#935 = CARTESIAN_POINT ( 'NONE',  ( -90.08403291566611415, -27.64547812922793923, -79.99999999999998579 ) ) ;
#936 = VERTEX_POINT ( 'NONE', #3385 ) ;
#937 = LINE ( 'NONE', #1390, #2653 ) ;
#938 = ORIENTED_EDGE ( 'NONE', *, *, #3903, .T. ) ;
#939 = CARTESIAN_POINT ( 'NONE',  ( -15.00000000000000178, 52.91502622129182498, 20.00000000000000000 ) ) ;
#940 = FACE_OUTER_BOUND ( 'NONE', #2415, .T. ) ;
#941 = DIRECTION ( 'NONE',  ( -0.7787725926866080339, -0.6273063437270329779, 0.000000000000000000 ) ) ;
#942 = ORIENTED_EDGE ( 'NONE', *, *, #895, .F. ) ;
#943 = CARTESIAN_POINT ( 'NONE',  ( 11.66987820548568600, -8.950926204225938321, 38.09167945787535103 ) ) ;
#944 = CARTESIAN_POINT ( 'NONE',  ( 8.432782529159780438, -9.370308598635425312, 25.44727941985334851 ) ) ;
#945 = VERTEX_POINT ( 'NONE', #1038 ) ;
#946 = EDGE_CURVE ( 'NONE', #656, #5782, #1457, .T. ) ;
#947 = EDGE_LOOP ( 'NONE', ( #1531, #1314, #3935, #3872, #5576 ) ) ;
#948 = LINE ( 'NONE', #2335, #4654 ) ;
#949 = DIRECTION ( 'NONE',  ( -0.000000000000000000, -0.000000000000000000, -1.000000000000000000 ) ) ;
#950 = LINE ( 'NONE', #2871, #1656 ) ;
#951 = DIRECTION ( 'NONE',  ( 1.000000000000000000, 0.000000000000000000, 0.000000000000000000 ) ) ;
#952 = DIRECTION ( 'NONE',  ( 1.000000000000000000, 0.000000000000000000, 0.000000000000000000 ) ) ;
#953 = DIRECTION ( 'NONE',  ( 0.6273063437270329779, -0.7787725926866080339, 0.000000000000000000 ) ) ;
#954 = AXIS2_PLACEMENT_3D ( 'NONE', #2303, #2213, #1775 ) ;
#955 = ORIENTED_EDGE ( 'NONE', *, *, #646, .F. ) ;
#956 = CARTESIAN_POINT ( 'NONE',  ( 8.830123324796599503E-15, 13.77854189090673742, 35.81030296219172726 ) ) ;
#957 = CARTESIAN_POINT ( 'NONE',  ( 9.958856949317492990, 8.309552794738946702, 22.73823205004162418 ) ) ;
#958 = CARTESIAN_POINT ( 'NONE',  ( 15.00000000000000178, 52.91502622129182498, 20.00000000000000000 ) ) ;
#959 = EDGE_CURVE ( 'NONE', #5881, #2218, #481, .T. ) ;
#960 = VECTOR ( 'NONE', #1277, 1000.000000000000227 ) ;
#961 = EDGE_CURVE ( 'NONE', #3596, #5854, #2473, .T. ) ;
#962 = VERTEX_POINT ( 'NONE', #5325 ) ;
#963 = CARTESIAN_POINT ( 'NONE',  ( -55.48030965892933608, -45.89047003626479437, 35.00000000000000000 ) ) ;
#964 = CIRCLE ( 'NONE', #5624, 5.141101056459331353 ) ;
#965 = AXIS2_PLACEMENT_3D ( 'NONE', #2285, #3254, #4203 ) ;
#966 = CARTESIAN_POINT ( 'NONE',  ( -10.23352841777491840, -8.662324224478982870, 30.54531597708798074 ) ) ;
#967 = DIRECTION ( 'NONE',  ( 1.000000000000000000, 0.000000000000000000, 0.000000000000000000 ) ) ;
#968 = ADVANCED_FACE ( 'NONE', ( #1075 ), #3257, .T. ) ;
#969 = AXIS2_PLACEMENT_3D ( 'NONE', #3897, #4783, #3342 ) ;
#970 = PRODUCT ( 'Die', 'Die', '', ( #2146 ) ) ;
#971 = CARTESIAN_POINT ( 'NONE',  ( 0.000000000000000000, 89.46264649666795776, -40.00000000000000000 ) ) ;
#972 = AXIS2_PLACEMENT_3D ( 'NONE', #529, #5210, #20 ) ;
#973 = CARTESIAN_POINT ( 'NONE',  ( 5.161660887237665918, -13.74708875321000789, 38.15586426248330554 ) ) ;
#974 = ORIENTED_EDGE ( 'NONE', *, *, #504, .T. ) ;
#975 = CARTESIAN_POINT ( 'NONE',  ( 67.48246767247886169, -25.10212255632678691, 35.00000000000000000 ) ) ;
#976 = VECTOR ( 'NONE', #3280, 999.9999999999998863 ) ;
#977 = ADVANCED_FACE ( 'NONE', ( #2013 ), #4384, .F. ) ;
#978 = DIRECTION ( 'NONE',  ( 1.000000000000000000, 0.000000000000000000, 0.000000000000000000 ) ) ;
#979 = CARTESIAN_POINT ( 'NONE',  ( 58.45671475544962448, 33.75000000000001421, 35.00000000000000000 ) ) ;
#980 = ORIENTED_EDGE ( 'NONE', *, *, #1593, .T. ) ;
#981 = DIRECTION ( 'NONE',  ( -0.000000000000000000, -0.000000000000000000, -1.000000000000000000 ) ) ;
#982 = AXIS2_PLACEMENT_3D ( 'NONE', #2154, #3583, #5500 ) ;
#983 = CARTESIAN_POINT ( 'NONE',  ( 3.759289558891017347, -12.45812449473959127, 33.24069098933200195 ) ) ;
#984 = ORIENTED_EDGE ( 'NONE', *, *, #4331, .T. ) ;
#985 = ORIENTED_EDGE ( 'NONE', *, *, #3040, .T. ) ;
#986 = DIRECTION ( 'NONE',  ( 0.000000000000000000, 1.000000000000000000, -0.000000000000000000 ) ) ;
#987 = CARTESIAN_POINT ( 'NONE',  ( 4.130675435985391572E-14, 1.067806758184284836E-13, -35.00000000000000000 ) ) ;
#988 = FACE_OUTER_BOUND ( 'NONE', #1209, .T. ) ;
#989 = VECTOR ( 'NONE', #3356, 1000.000000000000000 ) ;
#990 = FACE_OUTER_BOUND ( 'NONE', #5026, .T. ) ;
#991 = CARTESIAN_POINT ( 'NONE',  ( 0.000000000000000000, 67.50000000000000000, 20.00000000000000000 ) ) ;
#992 = VECTOR ( 'NONE', #1588, 1000.000000000000000 ) ;
#993 = VERTEX_POINT ( 'NONE', #1338 ) ;
#994 = CARTESIAN_POINT ( 'NONE',  ( 4.666652649023724564, 12.24723121994938779, 33.22501677959694177 ) ) ;
#995 = AXIS2_PLACEMENT_3D ( 'NONE', #2420, #5267, #4 ) ;
#996 = CARTESIAN_POINT ( 'NONE',  ( -3.317157231508560677, 9.910574073276151807, 22.73823205004162418 ) ) ;
#997 = CARTESIAN_POINT ( 'NONE',  ( 0.000000000000000000, 67.50000000000000000, 19.00000000000001066 ) ) ;
#998 = ORIENTED_EDGE ( 'NONE', *, *, #5906, .F. ) ;
#999 = FACE_OUTER_BOUND ( 'NONE', #4574, .T. ) ;
#1000 = B_SPLINE_CURVE_WITH_KNOTS ( 'NONE', 3,
 ( #5349, #634, #3868, #1440 ),
 .UNSPECIFIED., .F., .F.,
 ( 4, 4 ),
 ( 0.000000000000000000, 0.001907370850886569132 ),
 .UNSPECIFIED. ) ;
#1001 = AXIS2_PLACEMENT_3D ( 'NONE', #5430, #3956, #3984 ) ;
#1002 = CARTESIAN_POINT ( 'NONE',  ( -9.618700053625529378, -10.13908112636437053, 30.46372964425718521 ) ) ;
#1003 = CARTESIAN_POINT ( 'NONE',  ( -6.666666666666693608, -9.999999999999998224, 23.00000000000000000 ) ) ;
#1004 = TOROIDAL_SURFACE ( 'NONE', #3270, 72.00000000000004263, 10.00000000000000000 ) ;
#1005 =( REPRESENTATION_RELATIONSHIP ('NONE','NONE', #4716, #82 ) REPRESENTATION_RELATIONSHIP_WITH_TRANSFORMATION ( #331 )SHAPE_REPRESENTATION_RELATIONSHIP( ) );
#1006 = EDGE_CURVE ( 'NONE', #5881, #6071, #4043, .T. ) ;
#1007 = LINE ( 'NONE', #474, #4657 ) ;
#1008 = CARTESIAN_POINT ( 'NONE',  ( -7.765009959109524296, -12.46305503907367829, 38.11687012676383546 ) ) ;
#1009 = ORIENTED_EDGE ( 'NONE', *, *, #1006, .T. ) ;
#1010 = DIRECTION ( 'NONE',  ( 1.000000000000000000, 0.000000000000000000, 0.000000000000000000 ) ) ;
#1011 = CARTESIAN_POINT ( 'NONE',  ( 12.49999999999999822, 67.50000000000000000, -19.00000000000000711 ) ) ;
#1012 = FILL_AREA_STYLE_COLOUR ( '', #265 ) ;
#1013 = VERTEX_POINT ( 'NONE', #3118 ) ;
#1014 = FACE_BOUND ( 'NONE', #3004, .T. ) ;
#1015 = ADVANCED_FACE ( 'NONE', ( #5059 ), #6079, .F. ) ;
#1016 = CARTESIAN_POINT ( 'NONE',  ( 7.393143600131246274, -12.01612071878465571, 35.69844150329611665 ) ) ;
#1017 = VERTEX_POINT ( 'NONE', #4611 ) ;
#1018 = DIRECTION ( 'NONE',  ( -1.000000000000000000, 0.000000000000000000, 0.000000000000000000 ) ) ;
#1019 = ORIENTED_EDGE ( 'NONE', *, *, #2970, .T. ) ;
#1020 = DIRECTION ( 'NONE',  ( 0.000000000000000000, 1.000000000000000000, 0.000000000000000000 ) ) ;
#1021 = CARTESIAN_POINT ( 'NONE',  ( -47.58482424179536707, 72.37680137756343868, -79.99999999999998579 ) ) ;
#1022 = DIRECTION ( 'NONE',  ( 1.000000000000000000, 0.000000000000000000, -0.000000000000000000 ) ) ;
#1023 = DIRECTION ( 'NONE',  ( 1.000000000000000000, 0.000000000000000000, 0.000000000000000000 ) ) ;
#1024 = LINE ( 'NONE', #5212, #2674 ) ;
#1025 = DIRECTION ( 'NONE',  ( 0.000000000000000000, -1.000000000000000000, 0.000000000000000000 ) ) ;
#1026 = ORIENTED_EDGE ( 'NONE', *, *, #4032, .T. ) ;
#1027 = CARTESIAN_POINT ( 'NONE',  ( 3.080172029080881894E-14, 10.89081796499577237, 28.17941898721253580 ) ) ;
#1028 = CARTESIAN_POINT ( 'NONE',  ( -1.657983872361815658, 9.902916272933978803, 22.73823205004162418 ) ) ;
#1029 = DIRECTION ( 'NONE',  ( 0.000000000000000000, -0.000000000000000000, -1.000000000000000000 ) ) ;
#1030 = ORIENTED_EDGE ( 'NONE', *, *, #4531, .T. ) ;
#1031 = DIRECTION ( 'NONE',  ( -0.000000000000000000, -0.000000000000000000, -1.000000000000000000 ) ) ;
#1032 = CARTESIAN_POINT ( 'NONE',  ( -12.01612071878465393, -7.393143600131249826, 35.69844150329610954 ) ) ;
#1033 = CARTESIAN_POINT ( 'NONE',  ( -5.809855716632679190, -9.930636381741159369, 22.73823205004162773 ) ) ;
#1034 = CARTESIAN_POINT ( 'NONE',  ( -9.306281718482047438, 9.306281718482050991, 25.54332486258997292 ) ) ;
#1035 = CARTESIAN_POINT ( 'NONE',  ( -4.735139425639592226, -13.92517021172167624, 38.16137691020122702 ) ) ;
#1036 = EDGE_LOOP ( 'NONE', ( #3545, #2131, #2003, #343 ) ) ;
#1037 = CARTESIAN_POINT ( 'NONE',  ( -9.999999999999998224, -9.999999999999998224, -167.0000000000000284 ) ) ;
#1038 = CARTESIAN_POINT ( 'NONE',  ( -12.00000000000000000, 50.91502622129181788, 20.00000000000000000 ) ) ;
#1039 = EDGE_CURVE ( 'NONE', #5910, #413, #4673, .T. ) ;
#1040 = ADVANCED_FACE ( 'NONE', ( #2741 ), #363, .F. ) ;
#1041 = CARTESIAN_POINT ( 'NONE',  ( 57.58482424179591419, -72.37680137756305498, -40.00000000000000000 ) ) ;
#1042 = VERTEX_POINT ( 'NONE', #3696 ) ;
#1043 = FACE_BOUND ( 'NONE', #1489, .T. ) ;
#1044 = CARTESIAN_POINT ( 'NONE',  ( 5.845970755595360835, -13.50805179034379400, 38.28811402100272687 ) ) ;
#1045 = EDGE_LOOP ( 'NONE', ( #1790, #4583, #2088, #3942, #117, #3049 ) ) ;
#1046 = VERTEX_POINT ( 'NONE', #4140 ) ;
#1047 = FACE_OUTER_BOUND ( 'NONE', #5958, .T. ) ;
#1048 = CARTESIAN_POINT ( 'NONE',  ( 56.07162667343639839, -45.16605674834566742, 45.00000000000000711 ) ) ;
#1049 = DIRECTION ( 'NONE',  ( -0.7071067811865469066, -0.7071067811865482389, 0.000000000000000000 ) ) ;
#1050 = CARTESIAN_POINT ( 'NONE',  ( 88.34199753036777736, 94.27371331522249420, 0.000000000000000000 ) ) ;
#1051 = EDGE_CURVE ( 'NONE', #1654, #5395, #2655, .T. ) ;
#1052 = CARTESIAN_POINT ( 'NONE',  ( 55.48030965892933608, 45.89047003626479437, 35.00000000000000000 ) ) ;
#1053 = CARTESIAN_POINT ( 'NONE',  ( 9.977717576970368540, -7.732441893382042686, 28.03187055541259909 ) ) ;
#1054 = ORIENTED_EDGE ( 'NONE', *, *, #504, .F. ) ;
#1055 = ORIENTED_EDGE ( 'NONE', *, *, #1408, .F. ) ;
#1056 = CARTESIAN_POINT ( 'NONE',  ( 1.968046268140572819, 13.68733454931619775, 35.80501179064255268 ) ) ;
#1057 = CARTESIAN_POINT ( 'NONE',  ( -1.082228759108214478, 15.67638808697554786, 38.00000000000000711 ) ) ;
#1058 = CYLINDRICAL_SURFACE ( 'NONE', #6124, 5.000000000000004441 ) ;
#1059 = ADVANCED_FACE ( 'NONE', ( #395 ), #2240, .F. ) ;
#1060 = VECTOR ( 'NONE', #5434, 1000.000000000000000 ) ;
#1061 = ORIENTED_EDGE ( 'NONE', *, *, #5883, .T. ) ;
#1062 = DIRECTION ( 'NONE',  ( -1.000000000000000000, 0.000000000000000000, 0.000000000000000000 ) ) ;
#1063 = CARTESIAN_POINT ( 'NONE',  ( -13.77854189090673742, -0.9833031778629152120, 35.81030296219172726 ) ) ;
#1064 = AXIS2_PLACEMENT_3D ( 'NONE', #3822, #1156, #1865 ) ;
#1065 = ORIENTED_EDGE ( 'NONE', *, *, #5850, .F. ) ;
#1066 = CIRCLE ( 'NONE', #860, 80.00000000000000000 ) ;
#1067 = CARTESIAN_POINT ( 'NONE',  ( 9.166666666666657193, -9.999999999999998224, 23.00000000000000000 ) ) ;
#1068 = AXIS2_PLACEMENT_3D ( 'NONE', #2222, #6038, #3656 ) ;
#1069 = CIRCLE ( 'NONE', #2550, 80.00000000000000000 ) ;
#1070 = CARTESIAN_POINT ( 'NONE',  ( 8.999999999999998224, 8.999999999999998224, 23.00000000000000000 ) ) ;
#1071 = DIRECTION ( 'NONE',  ( 0.000000000000000000, 0.000000000000000000, -1.000000000000000000 ) ) ;
#1072 = AXIS2_PLACEMENT_3D ( 'NONE', #4812, #2443, #4303 ) ;
#1073 = ORIENTED_EDGE ( 'NONE', *, *, #2636, .T. ) ;
#1074 = CARTESIAN_POINT ( 'NONE',  ( 57.58482424179643999, 72.37680137756268550, -79.99999999999998579 ) ) ;
#1075 = FACE_OUTER_BOUND ( 'NONE', #5391, .T. ) ;
#1076 =( NAMED_UNIT ( * ) SI_UNIT ( $, .STERADIAN. ) SOLID_ANGLE_UNIT ( ) );
#1077 = VERTEX_POINT ( 'NONE', #3725 ) ;
#1078 = CARTESIAN_POINT ( 'NONE',  ( 12.00000000000000000, 50.91502622129181788, 20.00000000000000000 ) ) ;
#1079 = CARTESIAN_POINT ( 'NONE',  ( 5.819383256046889663, -8.963566061094551785, 22.99383858586043772 ) ) ;
#1080 = AXIS2_PLACEMENT_3D ( 'NONE', #2782, #2961, #1018 ) ;
#1081 = EDGE_CURVE ( 'NONE', #1820, #382, #1825, .T. ) ;
#1082 = ORIENTED_EDGE ( 'NONE', *, *, #1930, .F. ) ;
#1083 = ORIENTED_EDGE ( 'NONE', *, *, #4408, .F. ) ;
#1084 = CARTESIAN_POINT ( 'NONE',  ( 10.54244016040620835, -10.54244016040621190, 30.50000000000000000 ) ) ;
#1085 = DIRECTION ( 'NONE',  ( -0.3607836771741652626, 0.9326495259660446679, 0.000000000000000000 ) ) ;
#1086 = DIRECTION ( 'NONE',  ( 0.000000000000000000, 0.000000000000000000, 1.000000000000000000 ) ) ;
#1087 = PLANE ( 'NONE',  #2380 ) ;
#1088 = CARTESIAN_POINT ( 'NONE',  ( 0.000000000000000000, 50.91502622129181788, 20.00000000000000000 ) ) ;
#1089 = EDGE_CURVE ( 'NONE', #328, #5376, #1799, .T. ) ;
#1090 = AXIS2_PLACEMENT_3D ( 'NONE', #2994, #715, #5927 ) ;
#1091 = EDGE_LOOP ( 'NONE', ( #4998, #5006, #372, #5083 ) ) ;
#1092 = CARTESIAN_POINT ( 'NONE',  ( 5.113933401365548193, 9.708537589994000072, 25.56820946177495557 ) ) ;
#1093 = DIRECTION ( 'NONE',  ( -0.000000000000000000, -0.000000000000000000, 1.000000000000000000 ) ) ;
#1094 = DIRECTION ( 'NONE',  ( 1.000000000000000000, 0.000000000000000000, 0.000000000000000000 ) ) ;
#1095 = EDGE_LOOP ( 'NONE', ( #5196, #583, #892, #2898 ) ) ;
#1096 = DIRECTION ( 'NONE',  ( -0.000000000000000000, 0.000000000000000000, 1.000000000000000000 ) ) ;
#1097 = VECTOR ( 'NONE', #832, 1000.000000000000000 ) ;
#1098 = EDGE_CURVE ( 'NONE', #945, #1834, #307, .T. ) ;
#1099 = CARTESIAN_POINT ( 'NONE',  ( -13.33506331686137614, -3.878911688431557536, 35.78373290693654951 ) ) ;
#1100 = VECTOR ( 'NONE', #2822, 999.9999999999998863 ) ;
#1101 = ORIENTED_EDGE ( 'NONE', *, *, #5455, .T. ) ;
#1102 = VECTOR ( 'NONE', #5245, 1000.000000000000000 ) ;
#1103 = CARTESIAN_POINT ( 'NONE',  ( 9.696021465980065202, -12.35760627049922356, 37.99999999999999289 ) ) ;
#1104 = CIRCLE ( 'NONE', #710, 9.999999999999992895 ) ;
#1105 = CARTESIAN_POINT ( 'NONE',  ( 14.42236408824967242, 3.019346778933472031, 38.33740271606986738 ) ) ;
#1106 = DIRECTION ( 'NONE',  ( 0.7071067811865524577, 8.659560562354994488E-17, -0.7071067811865426878 ) ) ;
#1107 = AXIS2_PLACEMENT_3D ( 'NONE', #4269, #3765, #952 ) ;
#1108 = ORIENTED_EDGE ( 'NONE', *, *, #3013, .T. ) ;
#1109 = CARTESIAN_POINT ( 'NONE',  ( -55.00000000000010658, 21.27605460799956205, -35.00000000000000000 ) ) ;
#1110 = DIRECTION ( 'NONE',  ( 0.000000000000000000, 1.000000000000000000, 0.000000000000000000 ) ) ;
#1111 = CARTESIAN_POINT ( 'NONE',  ( 1.716690548177164821, -9.908812100099977371, 25.63028262842344773 ) ) ;
#1112 = ORIENTED_EDGE ( 'NONE', *, *, #48, .F. ) ;
#1113 = ORIENTED_EDGE ( 'NONE', *, *, #2696, .T. ) ;
#1114 = CARTESIAN_POINT ( 'NONE',  ( 10.72018218391672661, 10.03536489533503762, 38.06196296973745774 ) ) ;
#1115 = DIRECTION ( 'NONE',  ( 1.000000000000000000, 0.000000000000000000, 0.000000000000000000 ) ) ;
#1116 = CARTESIAN_POINT ( 'NONE',  ( 9.999999999999998224, 9.999999999999998224, -167.0000000000000284 ) ) ;
#1117 = ORIENTED_EDGE ( 'NONE', *, *, #3706, .F. ) ;
#1118 = EDGE_LOOP ( 'NONE', ( #158, #442, #3485, #918 ) ) ;
#1119 = CARTESIAN_POINT ( 'NONE',  ( 6.925743867604852610, 10.16167434176051643, 28.06532504456334109 ) ) ;
#1120 = CARTESIAN_POINT ( 'NONE',  ( 9.999999999999998224, -9.166666666666673180, 23.00000000000000000 ) ) ;
#1121 = DIRECTION ( 'NONE',  ( -0.8660254037844374864, -0.5000000000000018874, 0.000000000000000000 ) ) ;
#1122 = ADVANCED_FACE ( 'NONE', ( #2775 ), #6053, .T. ) ;
#1123 = EDGE_CURVE ( 'NONE', #4796, #1042, #2187, .T. ) ;
#1124 = EDGE_LOOP ( 'NONE', ( #3007, #2372, #4915, #1849 ) ) ;
#1125 = CARTESIAN_POINT ( 'NONE',  ( 0.000000000000000000, 0.000000000000000000, 45.00000000000000711 ) ) ;
#1126 = CARTESIAN_POINT ( 'NONE',  ( -9.708537589994000072, -5.113933401365464704, 25.56820946177495912 ) ) ;
#1127 = ORIENTED_EDGE ( 'NONE', *, *, #3568, .T. ) ;
#1128 = CARTESIAN_POINT ( 'NONE',  ( -9.696021465980074083, -12.35760627049922178, 38.00000000000000000 ) ) ;
#1129 = EDGE_CURVE ( 'NONE', #5138, #4037, #1779, .T. ) ;
#1130 = CARTESIAN_POINT ( 'NONE',  ( 13.90079966151757951, 4.954970571217797826, 38.30990426830500439 ) ) ;
#1131 = ORIENTED_EDGE ( 'NONE', *, *, #5292, .T. ) ;
#1132 = DIRECTION ( 'NONE',  ( 0.8660254037844385966, -0.5000000000000001110, 0.000000000000000000 ) ) ;
#1133 = DIRECTION ( 'NONE',  ( 1.000000000000000000, 0.000000000000000000, 0.000000000000000000 ) ) ;
#1134 = CARTESIAN_POINT ( 'NONE',  ( -2.763109891354090380E-14, -11.85339260696609465, 30.72304697887227221 ) ) ;
#1135 = VERTEX_POINT ( 'NONE', #337 ) ;
#1136 = DIRECTION ( 'NONE',  ( 0.000000000000000000, 0.000000000000000000, -1.000000000000000000 ) ) ;
#1137 = EDGE_LOOP ( 'NONE', ( #4292, #4354, #2571, #1131 ) ) ;
#1138 = CARTESIAN_POINT ( 'NONE',  ( -8.999999999999998224, 8.999999999999998224, -167.0000000000000284 ) ) ;
#1139 = LINE ( 'NONE', #3020, #3162 ) ;
#1140 = CONTEXT_DEPENDENT_SHAPE_REPRESENTATION ( #3099, #5831 ) ;
#1141 = CYLINDRICAL_SURFACE ( 'NONE', #1376, 5.000000000000005329 ) ;
#1142 = DIRECTION ( 'NONE',  ( 0.000000000000000000, 0.000000000000000000, 1.000000000000000000 ) ) ;
#1143 = ORIENTED_EDGE ( 'NONE', *, *, #1123, .T. ) ;
#1144 = CARTESIAN_POINT ( 'NONE',  ( 10.13908112636436343, 9.618700053625531154, 30.46372964425718521 ) ) ;
#1145 = CARTESIAN_POINT ( 'NONE',  ( 9.999999999999998224, -8.333333333333348136, 23.00000000000000000 ) ) ;
#1146 = EDGE_LOOP ( 'NONE', ( #4649, #2011, #4947, #457, #71 ) ) ;
#1147 = CARTESIAN_POINT ( 'NONE',  ( -11.42333844578496915, -4.533051537554476873, 30.68084101284746623 ) ) ;
#1148 = ORIENTED_EDGE ( 'NONE', *, *, #605, .F. ) ;
#1149 = EDGE_CURVE ( 'NONE', #2239, #2101, #505, .T. ) ;
#1150 = EDGE_CURVE ( 'NONE', #2322, #6134, #4456, .T. ) ;
#1151 = FACE_OUTER_BOUND ( 'NONE', #4461, .T. ) ;
#1152 = VECTOR ( 'NONE', #80, 1000.000000000000000 ) ;
#1153 = AXIS2_PLACEMENT_3D ( 'NONE', #5021, #769, #2651 ) ;
#1154 = CARTESIAN_POINT ( 'NONE',  ( 10.67327843797381171, 8.785602912694963962, 33.09221060678261495 ) ) ;
#1155 = EDGE_CURVE ( 'NONE', #4960, #3906, #3068, .T. ) ;
#1156 = DIRECTION ( 'NONE',  ( 0.000000000000000000, 0.000000000000000000, 1.000000000000000000 ) ) ;
#1157 = VERTEX_POINT ( 'NONE', #3209 ) ;
#1158 = LINE ( 'NONE', #2987, #1257 ) ;
#1159 = DIRECTION ( 'NONE',  ( 1.000000000000000000, 0.000000000000000000, 0.000000000000000000 ) ) ;
#1160 = CARTESIAN_POINT ( 'NONE',  ( -4.721144251037624463E-14, -8.965668681055127820, 23.09216300389307364 ) ) ;
#1161 = AXIS2_PLACEMENT_3D ( 'NONE', #3524, #3586, #191 ) ;
#1162 = EDGE_CURVE ( 'NONE', #3749, #1654, #5740, .T. ) ;
#1163 = ORIENTED_EDGE ( 'NONE', *, *, #3170, .F. ) ;
#1164 = DIRECTION ( 'NONE',  ( -1.000000000000000000, 0.000000000000000000, 0.000000000000000000 ) ) ;
#1165 = VERTEX_POINT ( 'NONE', #5776 ) ;
#1166 = DIRECTION ( 'NONE',  ( -1.000000000000000000, 0.000000000000000000, 0.000000000000000000 ) ) ;
#1167 = CYLINDRICAL_SURFACE ( 'NONE', #400, 2.499999999999998668 ) ;
#1168 = AXIS2_PLACEMENT_3D ( 'NONE', #1897, #5248, #1995 ) ;
#1169 = CARTESIAN_POINT ( 'NONE',  ( -27.50000000000010303, 47.63139720814406530, -35.00000000000000000 ) ) ;
#1170 = CYLINDRICAL_SURFACE ( 'NONE', #1867, 5.000000000000004441 ) ;
#1171 = ORIENTED_EDGE ( 'NONE', *, *, #3645, .F. ) ;
#1172 = ORIENTED_EDGE ( 'NONE', *, *, #582, .F. ) ;
#1173 = CARTESIAN_POINT ( 'NONE',  ( 9.086997423426605991, 11.58116666691846852, 38.17633527770230017 ) ) ;
#1174 = CARTESIAN_POINT ( 'NONE',  ( 9.999999999999998224, -4.166666666666706931, 23.00000000000000000 ) ) ;
#1175 = ORIENTED_EDGE ( 'NONE', *, *, #5364, .T. ) ;
#1176 = DIRECTION ( 'NONE',  ( -0.000000000000000000, -0.000000000000000000, -1.000000000000000000 ) ) ;
#1177 = CARTESIAN_POINT ( 'NONE',  ( -10.70751606408958700, -3.531709963121627105, 28.15279306126447523 ) ) ;
#1178 = VERTEX_POINT ( 'NONE', #5278 ) ;
#1179 = DIRECTION ( 'NONE',  ( -0.000000000000000000, -0.000000000000000000, -1.000000000000000000 ) ) ;
#1180 = AXIS2_PLACEMENT_3D ( 'NONE', #837, #5115, #862 ) ;
#1181 = AXIS2_PLACEMENT_3D ( 'NONE', #102, #4254, #5793 ) ;
#1182 = CARTESIAN_POINT ( 'NONE',  ( 8.963566061094550008, 5.819383256046893216, 22.99383858586042351 ) ) ;
#1183 = AXIS2_PLACEMENT_3D ( 'NONE', #4482, #4422, #2054 ) ;
#1184 = DIRECTION ( 'NONE',  ( -0.000000000000000000, 0.000000000000000000, 1.000000000000000000 ) ) ;
#1185 = VERTEX_POINT ( 'NONE', #3365 ) ;
#1186 = CARTESIAN_POINT ( 'NONE',  ( -9.000000000000005329, 8.999999999988014920, 23.06137295785748265 ) ) ;
#1187 = AXIS2_PLACEMENT_3D ( 'NONE', #4904, #683, #5898 ) ;
#1188 = EDGE_CURVE ( 'NONE', #404, #1798, #2373, .T. ) ;
#1189 = LINE ( 'NONE', #3046, #1580 ) ;
#1190 = CIRCLE ( 'NONE', #1107, 11.50000000000000355 ) ;
#1191 = CARTESIAN_POINT ( 'NONE',  ( -0.9833031778629336417, -13.77854189090673742, 35.81030296219173437 ) ) ;
#1192 = ORIENTED_EDGE ( 'NONE', *, *, #2118, .F. ) ;
#1193 = CARTESIAN_POINT ( 'NONE',  ( -46.52501622030217021, -37.47620048660763103, 35.00000000000000000 ) ) ;
#1194 = VERTEX_POINT ( 'NONE', #4324 ) ;
#1195 = DIRECTION ( 'NONE',  ( -0.000000000000000000, 0.000000000000000000, 1.000000000000000000 ) ) ;
#1196 = DIRECTION ( 'NONE',  ( -0.000000000000000000, -0.000000000000000000, -1.000000000000000000 ) ) ;
#1197 = ITEM_DEFINED_TRANSFORMATION ( 'NONE', 'NONE', #782,  #73 ) ;
#1198 = EDGE_CURVE ( 'NONE', #4858, #2502, #2371, .T. ) ;
#1199 = DIRECTION ( 'NONE',  ( 1.000000000000000000, 0.000000000000000000, 0.000000000000000000 ) ) ;
#1200 = EDGE_CURVE ( 'NONE', #4821, #705, #948, .T. ) ;
#1201 = LINE ( 'NONE', #4042, #899 ) ;
#1202 = VERTEX_POINT ( 'NONE', #3330 ) ;
#1203 = CARTESIAN_POINT ( 'NONE',  ( 8.539139919159236314, 9.793760812180218878, 27.99841606626185353 ) ) ;
#1204 = CARTESIAN_POINT ( 'NONE',  ( 12.35760627049921823, -9.696021465980074083, 38.00000000000000000 ) ) ;
#1205 = PLANE ( 'NONE',  #3442 ) ;
#1206 = ORIENTED_EDGE ( 'NONE', *, *, #4650, .F. ) ;
#1207 = CARTESIAN_POINT ( 'NONE',  ( 99.00000000000005684, 1.218523565151616775E-14, 40.00000000000000000 ) ) ;
#1208 = CARTESIAN_POINT ( 'NONE',  ( -11.58281169573755953, 3.645573174172184405, 30.69674159737795449 ) ) ;
#1209 = EDGE_LOOP ( 'NONE', ( #1696, #440, #232, #3423 ) ) ;
#1210 = DIRECTION ( 'NONE',  ( -0.000000000000000000, -0.000000000000000000, 1.000000000000000000 ) ) ;
#1211 = PRODUCT_RELATED_PRODUCT_CATEGORY ( 'part', '', ( #825 ) ) ;
#1212 = CARTESIAN_POINT ( 'NONE',  ( 9.793778397576030414, 8.539045536263008884, 27.99842134739334654 ) ) ;
#1213 = ORIENTED_EDGE ( 'NONE', *, *, #2517, .T. ) ;
#1214 = CARTESIAN_POINT ( 'NONE',  ( -6.666666666666638541, 9.999999999999998224, 23.00000000000000000 ) ) ;
#1215 = LINE ( 'NONE', #5487, #3074 ) ;
#1216 = CARTESIAN_POINT ( 'NONE',  ( -1.968046268140571486, -13.68733454931619953, 35.80501179064255268 ) ) ;
#1217 = ORIENTED_EDGE ( 'NONE', *, *, #432, .T. ) ;
#1218 = CARTESIAN_POINT ( 'NONE',  ( -11.33314185116958051, 72.77350886804100583, 35.00000000000000000 ) ) ;
#1219 = ORIENTED_EDGE ( 'NONE', *, *, #5913, .T. ) ;
#1220 = DIRECTION ( 'NONE',  ( -0.000000000000000000, -0.000000000000000000, -1.000000000000000000 ) ) ;
#1221 = ADVANCED_FACE ( 'NONE', ( #490 ), #3821, .T. ) ;
#1222 = EDGE_CURVE ( 'NONE', #3173, #149, #5703, .T. ) ;
#1223 = CARTESIAN_POINT ( 'NONE',  ( 0.000000000000000000, 0.000000000000000000, 35.00000000000000000 ) ) ;
#1224 = CARTESIAN_POINT ( 'NONE',  ( 5.000000000000003553, 89.46264649666795776, -40.00000000000000000 ) ) ;
#1225 = CARTESIAN_POINT ( 'NONE',  ( -9.999999999999998224, -1.666666666666617225, 23.00000000000000000 ) ) ;
#1226 = ORIENTED_EDGE ( 'NONE', *, *, #3873, .T. ) ;
#1227 = DIRECTION ( 'NONE',  ( 0.000000000000000000, -1.000000000000000000, 0.000000000000000000 ) ) ;
#1228 = EDGE_CURVE ( 'NONE', #1202, #2489, #17, .T. ) ;
#1229 = LINE ( 'NONE', #4014, #5612 ) ;
#1230 = CARTESIAN_POINT ( 'NONE',  ( 9.999999999999998224, -3.333333333333376558, 23.00000000000000000 ) ) ;
#1231 = DIRECTION ( 'NONE',  ( 0.000000000000000000, -1.000000000000000000, 0.000000000000000000 ) ) ;
#1232 = ORIENTED_EDGE ( 'NONE', *, *, #5079, .F. ) ;
#1233 = CARTESIAN_POINT ( 'NONE',  ( -13.33504572891042272, 3.879012780925821247, 35.78373437249953781 ) ) ;
#1234 = ORIENTED_EDGE ( 'NONE', *, *, #3885, .T. ) ;
#1235 = ADVANCED_FACE ( 'NONE', ( #1047 ), #4774, .T. ) ;
#1236 = DIRECTION ( 'NONE',  ( 0.000000000000000000, 0.000000000000000000, -1.000000000000000000 ) ) ;
#1237 = DIRECTION ( 'NONE',  ( -1.000000000000000000, 0.000000000000000000, 0.000000000000000000 ) ) ;
#1238 = CARTESIAN_POINT ( 'NONE',  ( 12.31015466235579225, -79.04720167209512738, -35.00000000000000000 ) ) ;
#1239 = ORIENTED_EDGE ( 'NONE', *, *, #827, .F. ) ;
#1240 = CARTESIAN_POINT ( 'NONE',  ( -8.159736356077658570, -11.57174281757876955, 35.66679457777021156 ) ) ;
#1241 = ORIENTED_EDGE ( 'NONE', *, *, #5676, .F. ) ;
#1242 = CARTESIAN_POINT ( 'NONE',  ( -8.999999999988011368, -9.000000000000007105, 23.06137295785747909 ) ) ;
#1243 = ORIENTED_EDGE ( 'NONE', *, *, #5448, .T. ) ;
#1244 = DIRECTION ( 'NONE',  ( 0.5000000000000101030, -0.8660254037844328234, 0.000000000000000000 ) ) ;
#1245 =( GEOMETRIC_REPRESENTATION_CONTEXT ( 3 ) GLOBAL_UNCERTAINTY_ASSIGNED_CONTEXT ( ( #4246 ) ) GLOBAL_UNIT_ASSIGNED_CONTEXT ( ( #1819, #3753, #10 ) ) REPRESENTATION_CONTEXT ( 'NONE', 'WORKASPACE' ) );
#1246 = DIRECTION ( 'NONE',  ( 0.7071067811865573427, 0.000000000000000000, 0.7071067811865378028 ) ) ;
#1247 = ITEM_DEFINED_TRANSFORMATION ( 'NONE', 'NONE', #3829,  #73 ) ;
#1248 = CARTESIAN_POINT ( 'NONE',  ( 52.91502622129182498, 15.00000000000001954, -35.00000000000000000 ) ) ;
#1249 = CARTESIAN_POINT ( 'NONE',  ( -9.999999999999998224, -5.833333333333296622, 23.00000000000000000 ) ) ;
#1250 = CIRCLE ( 'NONE', #269, 80.00000000000000000 ) ;
#1251 = ADVANCED_FACE ( 'NONE', ( #2404 ), #1402, .F. ) ;
#1252 = VERTEX_POINT ( 'NONE', #2925 ) ;
#1253 = DIRECTION ( 'NONE',  ( 0.000000000000000000, 1.000000000000000000, 0.000000000000000000 ) ) ;
#1254 = DIRECTION ( 'NONE',  ( 0.000000000000000000, -0.000000000000000000, -1.000000000000000000 ) ) ;
#1255 = CARTESIAN_POINT ( 'NONE',  ( 0.000000000000000000, 67.50000000000000000, 20.00000000000000000 ) ) ;
#1256 = CARTESIAN_POINT ( 'NONE',  ( 12.31015466235579581, -79.04720167209514159, 38.99999999999995737 ) ) ;
#1257 = VECTOR ( 'NONE', #229, 1000.000000000000000 ) ;
#1258 = ORIENTED_EDGE ( 'NONE', *, *, #4180, .F. ) ;
#1259 = CARTESIAN_POINT ( 'NONE',  ( 12.41448144607148052, -6.563799387313611788, 35.72511331161844339 ) ) ;
#1260 = EDGE_CURVE ( 'NONE', #4988, #4357, #802, .T. ) ;
#1261 = CARTESIAN_POINT ( 'NONE',  ( -9.778265677387498300, 4.273055220303942470, 25.59105958838676997 ) ) ;
#1262 = ORIENTED_EDGE ( 'NONE', *, *, #5100, .T. ) ;
#1263 = AXIS2_PLACEMENT_3D ( 'NONE', #509, #3316, #4204 ) ;
#1264 = FACE_BOUND ( 'NONE', #2991, .T. ) ;
#1265 = PLANE ( 'NONE',  #1544 ) ;
#1266 = EDGE_CURVE ( 'NONE', #1046, #4044, #5961, .T. ) ;
#1267 = PLANE ( 'NONE',  #4208 ) ;
#1268 = ORIENTED_EDGE ( 'NONE', *, *, #253, .T. ) ;
#1269 = AXIS2_PLACEMENT_3D ( 'NONE', #3631, #4666, #385 ) ;
#1270 = CARTESIAN_POINT ( 'NONE',  ( -9.157688896001754841, -8.975362584346067152, 22.85246612729343596 ) ) ;
#1271 = EDGE_LOOP ( 'NONE', ( #3181, #5939 ) ) ;
#1272 = FACE_BOUND ( 'NONE', #4669, .T. ) ;
#1273 = EDGE_LOOP ( 'NONE', ( #543, #808 ) ) ;
#1274 = LINE ( 'NONE', #5018, #5757 ) ;
#1275 = CARTESIAN_POINT ( 'NONE',  ( 0.000000000000000000, 50.91502622129181788, 35.00000000000000000 ) ) ;
#1276 = AXIS2_PLACEMENT_3D ( 'NONE', #5398, #3888, #2107 ) ;
#1277 = DIRECTION ( 'NONE',  ( 0.1538769332794487910, -0.9880900209011889146, 0.000000000000000000 ) ) ;
#1278 = PLANE ( 'NONE',  #1480 ) ;
#1279 = AXIS2_PLACEMENT_3D ( 'NONE', #239, #4513, #5930 ) ;
#1280 = DIRECTION ( 'NONE',  ( -0.000000000000000000, -0.000000000000000000, -1.000000000000000000 ) ) ;
#1281 = ORIENTED_EDGE ( 'NONE', *, *, #5948, .T. ) ;
#1282 = DIRECTION ( 'NONE',  ( 1.000000000000000000, 0.000000000000000000, 0.000000000000000000 ) ) ;
#1283 = PLANE ( 'NONE',  #3222 ) ;
#1284 = CIRCLE ( 'NONE', #1976, 15.67638808697555142 ) ;
#1285 = PRESENTATION_STYLE_ASSIGNMENT (( #3643 ) ) ;
#1286 = CARTESIAN_POINT ( 'NONE',  ( 10.89081796499577059, -3.519470773090535588E-14, 28.17941898721253580 ) ) ;
#1287 = CARTESIAN_POINT ( 'NONE',  ( -8.964120815521452457, 3.322922547535531734, 23.06129036953744915 ) ) ;
#1288 = VERTEX_POINT ( 'NONE', #3789 ) ;
#1289 = CARTESIAN_POINT ( 'NONE',  ( -4.154428044945160714, 8.963431230391419646, 23.04275563843252783 ) ) ;
#1290 = DIRECTION ( 'NONE',  ( -1.000000000000000000, -4.496403249731883200E-15, 0.000000000000000000 ) ) ;
#1291 = ADVANCED_FACE ( 'NONE', ( #2432 ), #3394, .T. ) ;
#1292 = ADVANCED_FACE ( 'NONE', ( #591 ), #2469, .F. ) ;
#1293 = CARTESIAN_POINT ( 'NONE',  ( 0.000000000000000000, 0.000000000000000000, 38.99999999999995737 ) ) ;
#1294 = DIRECTION ( 'NONE',  ( 1.000000000000000000, -0.000000000000000000, 0.000000000000000000 ) ) ;
#1295 = ADVANCED_FACE ( 'NONE', ( #1993 ), #4736, .T. ) ;
#1296 = FACE_OUTER_BOUND ( 'NONE', #11, .T. ) ;
#1297 = ADVANCED_FACE ( 'NONE', ( #2803 ), #609, .F. ) ;
#1298 = B_SPLINE_SURFACE_WITH_KNOTS ( 'NONE', 3, 3, ( 
 ( #5480, #752, #5039, #4056, #317, #2160, #5975 ),
 ( #785, #4498, #4563, #6000, #5536, #5446, #2098 ),
 ( #3528, #2752, #5590, #344, #1873, #904, #405 ),
 ( #928, #2345, #3245, #871, #1346, #1378, #2784 ),
 ( #3676, #4651, #3649, #4680, #3283, #3216, #3768 ),
 ( #5683, #6085, #5070, #817, #1836, #2693, #6062 ),
 ( #2281, #430, #3702, #843, #2309, #4591, #4199 ),
 ( #4235, #2219, #5187, #4110, #6032, #2810, #1289 ),
 ( #1782, #3251, #6115, #4706, #1806, #458, #5565 ),
 ( #1752, #3188, #2719, #5097, #4148, #4617, #2251 ),
 ( #374, #1315, #5123, #4173, #5156, #1968, #4369 ),
 ( #87, #562, #4810, #2441, #3831, #2936, #5810 ),
 ( #1932, #956, #4398, #2973, #1027, #5748, #4747 ),
 ( #5312, #4335, #1410, #5348, #632, #146, #5285 ),
 ( #1532, #1056, #50, #1474, #2906, #1902, #4848 ),
 ( #3372, #2027, #3926, #3310, #3866, #5218, #2842 ),
 ( #500, #4301, #2382, #5783, #599, #1504, #5253 ),
 ( #4273, #2479, #994, #2510, #25, #120, #3797 ),
 ( #3895, #5711, #3400, #2000, #3434, #1092, #4884 ),
 ( #1438, #3340, #2878, #4781, #534, #2412, #186 ),
 ( #2152, #4938, #4490, #5473, #1119, #1682, #2115 ),
 ( #5878, #689, #4516, #4430, #2061, #721, #272 ),
 ( #1173, #3062, #3119, #1595, #1203, #3092, #3491 ),
 ( #5000, #744, #3582, #4045, #243, #2625, #5966 ),
 ( #5404, #5499, #1618, #1144, #4910, #2656, #3467 ) ),
 .UNSPECIFIED., .F., .F., .F.,
 ( 4, 3, 3, 3, 3, 3, 3, 3, 4 ),
 ( 4, 3, 4 ),
 ( 0.000000000000000000, 0.1250000000000000000, 0.2500000000000000000, 0.3750000000000000000, 0.5000000000000000000, 0.6250000000000000000, 0.7500000000000000000, 0.8750000000000000000, 1.000000000000000000 ),
 ( 0.000000000000000000, 0.5087255983319458608, 1.017451196663891722 ),
 .UNSPECIFIED. ) ;
#1299 = LINE ( 'NONE', #850, #1763 ) ;
#1300 = EDGE_LOOP ( 'NONE', ( #5701, #608 ) ) ;
#1301 = DIRECTION ( 'NONE',  ( -1.000000000000000000, 0.000000000000000000, 0.000000000000000000 ) ) ;
#1302 = VERTEX_POINT ( 'NONE', #451 ) ;
#1303 = FACE_OUTER_BOUND ( 'NONE', #3931, .T. ) ;
#1304 = CARTESIAN_POINT ( 'NONE',  ( -9.999999999999998224, 9.999999999999998224, 23.00000000000000000 ) ) ;
#1305 = DIRECTION ( 'NONE',  ( -0.8660254037844385966, 0.5000000000000001110, 0.000000000000000000 ) ) ;
#1306 = CARTESIAN_POINT ( 'NONE',  ( -9.999999999999998224, 9.999999999999998224, 23.00000000000000000 ) ) ;
#1307 = PLANE ( 'NONE',  #3165 ) ;
#1308 = VERTEX_POINT ( 'NONE', #3084 ) ;
#1309 = DIRECTION ( 'NONE',  ( 0.4999999999999976685, 0.8660254037844400399, 0.000000000000000000 ) ) ;
#1310 = CARTESIAN_POINT ( 'NONE',  ( 57.58482424179643999, 72.37680137756268550, 40.00000000000000000 ) ) ;
#1311 = CARTESIAN_POINT ( 'NONE',  ( -10.37777353962637505, 10.37777353962536608, 38.05103295300745003 ) ) ;
#1312 = CARTESIAN_POINT ( 'NONE',  ( 9.928243323025453648, -2.905319074912632839E-14, 25.63579099555277807 ) ) ;
#1313 = CARTESIAN_POINT ( 'NONE',  ( -10.77715421822219177, 7.077172123266720405, 30.61076540981939687 ) ) ;
#1314 = ORIENTED_EDGE ( 'NONE', *, *, #3282, .T. ) ;
#1315 = CARTESIAN_POINT ( 'NONE',  ( -1.968147360634808329, 13.68731696136523546, 35.80501325620552677 ) ) ;
#1316 = CARTESIAN_POINT ( 'NONE',  ( 0.000000000000000000, 0.000000000000000000, -35.00000000000000000 ) ) ;
#1317 = CARTESIAN_POINT ( 'NONE',  ( -58.45671475544979501, 33.74999999999974420, -35.00000000000000000 ) ) ;
#1318 = EDGE_CURVE ( 'NONE', #5782, #1798, #5425, .T. ) ;
#1319 = DIRECTION ( 'NONE',  ( -0.1538769332794488187, 0.9880900209011889146, 0.000000000000000000 ) ) ;
#1320 = DIRECTION ( 'NONE',  ( 0.000000000000000000, 0.000000000000000000, -1.000000000000000000 ) ) ;
#1321 = PRODUCT_DEFINITION_CONTEXT ( 'detailed design', #161, 'design' ) ;
#1322 = EDGE_CURVE ( 'NONE', #4090, #3660, #703, .T. ) ;
#1323 = EDGE_CURVE ( 'NONE', #4821, #1077, #1612, .T. ) ;
#1324 = CARTESIAN_POINT ( 'NONE',  ( -5.247549479766072444, -10.46302782743270932, 28.11481907968152427 ) ) ;
#1325 = ORIENTED_EDGE ( 'NONE', *, *, #646, .T. ) ;
#1326 = CARTESIAN_POINT ( 'NONE',  ( -9.999999999999998224, -9.999999999999998224, 23.00000000000000000 ) ) ;
#1327 = ORIENTED_EDGE ( 'NONE', *, *, #130, .T. ) ;
#1328 = CARTESIAN_POINT ( 'NONE',  ( 14.67638808697554964, 1.797339169375895343E-15, 205.0000000000000568 ) ) ;
#1329 = LINE ( 'NONE', #5578, #1854 ) ;
#1330 = AXIS2_PLACEMENT_3D ( 'NONE', #3347, #1096, #1479 ) ;
#1331 = FACE_OUTER_BOUND ( 'NONE', #880, .T. ) ;
#1332 = CARTESIAN_POINT ( 'NONE',  ( -9.902916272933978803, 1.657983872361913358, 22.73823205004162418 ) ) ;
#1333 = EDGE_CURVE ( 'NONE', #4672, #2051, #2503, .T. ) ;
#1334 = LINE ( 'NONE', #1735, #95 ) ;
#1335 = VECTOR ( 'NONE', #338, 1000.000000000000000 ) ;
#1336 = VECTOR ( 'NONE', #3920, 1000.000000000000000 ) ;
#1337 = EDGE_LOOP ( 'NONE', ( #1724, #6116, #4750, #792 ) ) ;
#1338 = CARTESIAN_POINT ( 'NONE',  ( 47.58482424179590708, -72.37680137756305498, -40.00000000000000000 ) ) ;
#1339 = DIRECTION ( 'NONE',  ( 1.000000000000000000, 0.000000000000000000, 0.000000000000000000 ) ) ;
#1340 = DIRECTION ( 'NONE',  ( -1.000000000000000000, 0.000000000000000000, 0.000000000000000000 ) ) ;
#1341 = CIRCLE ( 'NONE', #2444, 80.00000000000000000 ) ;
#1342 = CARTESIAN_POINT ( 'NONE',  ( 10.78034266696900367, -2.654236408786761814, 28.16346921039841433 ) ) ;
#1343 = SURFACE_STYLE_FILL_AREA ( #2501 ) ;
#1344 = AXIS2_PLACEMENT_3D ( 'NONE', #1708, #3556, #2603 ) ;
#1345 = VERTEX_POINT ( 'NONE', #5925 ) ;
#1346 = CARTESIAN_POINT ( 'NONE',  ( -7.732441893382013376, 9.977717576970368540, 28.03187055541259198 ) ) ;
#1347 = DIRECTION ( 'NONE',  ( -0.000000000000000000, -0.000000000000000000, -1.000000000000000000 ) ) ;
#1348 = CIRCLE ( 'NONE', #2556, 55.00000000000001421 ) ;
#1349 = ORIENTED_EDGE ( 'NONE', *, *, #3088, .F. ) ;
#1350 = CARTESIAN_POINT ( 'NONE',  ( 8.999999999999992895, 3.000397777471232708, 23.18288458324510515 ) ) ;
#1351 = AXIS2_PLACEMENT_3D ( 'NONE', #3508, #4480, #5922 ) ;
#1352 = CARTESIAN_POINT ( 'NONE',  ( 15.67638808697555142, 1.919803849290630886E-15, 205.0000000000000568 ) ) ;
#1353 = DIRECTION ( 'NONE',  ( -0.000000000000000000, -0.000000000000000000, -1.000000000000000000 ) ) ;
#1354 = CLOSED_SHELL ( 'NONE', ( #476, #1295, #3315, #667, #2484, #4606, #2119, #4414, #4024, #468, #2528 ) ) ;
#1355 = CARTESIAN_POINT ( 'NONE',  ( 11.08488032081242380, 11.08488032081242025, 38.00000000000000000 ) ) ;
#1356 = AXIS2_PLACEMENT_3D ( 'NONE', #2406, #1085, #3791 ) ;
#1357 = PLANE ( 'NONE',  #1843 ) ;
#1358 = ORIENTED_EDGE ( 'NONE', *, *, #1857, .T. ) ;
#1359 = FACE_OUTER_BOUND ( 'NONE', #1337, .T. ) ;
#1360 = CARTESIAN_POINT ( 'NONE',  ( 0.000000000000000000, 0.000000000000000000, 39.00000000000007105 ) ) ;
#1361 = EDGE_CURVE ( 'NONE', #4312, #3660, #2619, .T. ) ;
#1362 = FILL_AREA_STYLE ('',( #1012 ) ) ;
#1363 = ORIENTED_EDGE ( 'NONE', *, *, #1913, .T. ) ;
#1364 = CARTESIAN_POINT ( 'NONE',  ( 13.37091851167925149, -6.070355506015043368, 38.14417062278695880 ) ) ;
#1365 = CONICAL_SURFACE ( 'NONE', #3654, 99.00000000000005684, 0.7853981633974552734 ) ;
#1366 = CARTESIAN_POINT ( 'NONE',  ( 0.000000000000000000, 67.50000000000000000, -19.00000000000000711 ) ) ;
#1367 = AXIS2_PLACEMENT_3D ( 'NONE', #1699, #5987, #6010 ) ;
#1368 = VERTEX_POINT ( 'NONE', #4961 ) ;
#1369 = DIRECTION ( 'NONE',  ( 1.000000000000000000, 0.000000000000000000, 0.000000000000000000 ) ) ;
#1370 = DIRECTION ( 'NONE',  ( 0.000000000000000000, 0.000000000000000000, 1.000000000000000000 ) ) ;
#1371 = EDGE_CURVE ( 'NONE', #3081, #1401, #4508, .T. ) ;
#1372 = CARTESIAN_POINT ( 'NONE',  ( 0.000000000000000000, 67.50000000000000000, 28.99999999999999645 ) ) ;
#1373 = EDGE_CURVE ( 'NONE', #4037, #1523, #4758, .T. ) ;
#1374 = CARTESIAN_POINT ( 'NONE',  ( -45.92560378283280187, -36.99336990414421678, 35.00000000000000000 ) ) ;
#1375 = CARTESIAN_POINT ( 'NONE',  ( 13.33504572891042095, -3.879012780925821691, 35.78373437249953781 ) ) ;
#1376 = AXIS2_PLACEMENT_3D ( 'NONE', #2596, #4395, #1199 ) ;
#1377 = ORIENTED_EDGE ( 'NONE', *, *, #4999, .T. ) ;
#1378 = CARTESIAN_POINT ( 'NONE',  ( -7.610208295502463471, 9.462636878983097688, 25.48187184588751464 ) ) ;
#1379 = ORIENTED_EDGE ( 'NONE', *, *, #2734, .T. ) ;
#1380 = DIRECTION ( 'NONE',  ( -0.6273063437270228748, -0.7787725926866162496, 0.000000000000000000 ) ) ;
#1381 = ORIENTED_EDGE ( 'NONE', *, *, #3194, .T. ) ;
#1382 = CARTESIAN_POINT ( 'NONE',  ( 68.69027832783777399, 26.57196568621521138, 35.13717928826270054 ) ) ;
#1383 = CARTESIAN_POINT ( 'NONE',  ( -9.166555234036119160, -10.04707028972859106, 25.36260747786040071 ) ) ;
#1384 = CARTESIAN_POINT ( 'NONE',  ( -62.30180741492871022, -50.18450749816254586, 35.00000000000000000 ) ) ;
#1385 = UNCERTAINTY_MEASURE_WITH_UNIT (LENGTH_MEASURE( 1.000000000000000082E-05 ), #5406, 'distance_accuracy_value', 'NONE');
#1386 = PRODUCT_DEFINITION_SHAPE ( 'NONE', 'NONE',  #6153 ) ;
#1387 = PRODUCT_DEFINITION ( 'UNKNOWN', '', #4631, #2453 ) ;
#1388 = CARTESIAN_POINT ( 'NONE',  ( 9.858401829237468661, 10.19494410001831675, 33.01259202755186095 ) ) ;
#1389 = EDGE_LOOP ( 'NONE', ( #5861, #91, #4233, #4006 ) ) ;
#1390 = CARTESIAN_POINT ( 'NONE',  ( 1.131281550719567528E-13, 1.761763928569687004E-14, 35.00000000000000000 ) ) ;
#1391 = EDGE_LOOP ( 'NONE', ( #76, #1113, #4616, #460 ) ) ;
#1392 = DIRECTION ( 'NONE',  ( -0.000000000000000000, -0.000000000000000000, -1.000000000000000000 ) ) ;
#1393 = CARTESIAN_POINT ( 'NONE',  ( 0.000000000000000000, 67.50000000000000000, -19.00000000000000000 ) ) ;
#1394 = CYLINDRICAL_SURFACE ( 'NONE', #4719, 5.000000000000003553 ) ;
#1395 = ORIENTED_EDGE ( 'NONE', *, *, #3668, .T. ) ;
#1396 = DIRECTION ( 'NONE',  ( 0.000000000000000000, 0.000000000000000000, 1.000000000000000000 ) ) ;
#1397 = CARTESIAN_POINT ( 'NONE',  ( 100.0000000000000000, 1.224646799147353217E-14, 39.00000000000007105 ) ) ;
#1398 = EDGE_CURVE ( 'NONE', #5460, #882, #4987, .T. ) ;
#1399 = EDGE_CURVE ( 'NONE', #1672, #3029, #3458, .T. ) ;
#1400 = ORIENTED_EDGE ( 'NONE', *, *, #1748, .T. ) ;
#1401 = VERTEX_POINT ( 'NONE', #1138 ) ;
#1402 = CYLINDRICAL_SURFACE ( 'NONE', #2971, 5.000000000000004441 ) ;
#1403 = CARTESIAN_POINT ( 'NONE',  ( -11.33314185116958051, 72.77350886804100583, 35.13717928826310555 ) ) ;
#1404 = PRODUCT ( 'Roller', 'Roller', '', ( #2650 ) ) ;
#1405 = CARTESIAN_POINT ( 'NONE',  ( 8.586443133426902668E-15, -8.586443133426886890E-15, 20.00000000000000000 ) ) ;
#1406 = CARTESIAN_POINT ( 'NONE',  ( -74.61196207728360719, -28.86269417393314995, 35.00000000000000000 ) ) ;
#1407 = CARTESIAN_POINT ( 'NONE',  ( 10.77715421822219355, -7.077172123266713299, 30.61076540981938976 ) ) ;
#1408 = EDGE_CURVE ( 'NONE', #1157, #2972, #2564, .T. ) ;
#1409 = EDGE_LOOP ( 'NONE', ( #5433, #2142, #3328, #3543 ) ) ;
#1410 = CARTESIAN_POINT ( 'NONE',  ( 0.9505942623812212444, 12.81596724893641337, 33.26667497053200151 ) ) ;
#1411 = DIRECTION ( 'NONE',  ( -8.673617379884026597E-16, -1.000000000000000000, 0.000000000000000000 ) ) ;
#1412 = FACE_OUTER_BOUND ( 'NONE', #3433, .T. ) ;
#1413 = EDGE_LOOP ( 'NONE', ( #5205, #2301, #5017, #1262 ) ) ;
#1414 = CARTESIAN_POINT ( 'NONE',  ( -5.141101056459331353, 67.50000000000000000, -28.99999999999999645 ) ) ;
#1415 = EDGE_CURVE ( 'NONE', #1915, #3734, #1664, .T. ) ;
#1416 = CARTESIAN_POINT ( 'NONE',  ( -9.370308598635419983, -8.432782529159780438, 25.44727941985334496 ) ) ;
#1417 = CARTESIAN_POINT ( 'NONE',  ( 11.08488032081241847, -11.08488032081242380, 38.00000000000000000 ) ) ;
#1418 =( REPRESENTATION_RELATIONSHIP ('NONE','NONE', #4716, #82 ) REPRESENTATION_RELATIONSHIP_WITH_TRANSFORMATION ( #3982 )SHAPE_REPRESENTATION_RELATIONSHIP( ) );
#1419 = CARTESIAN_POINT ( 'NONE',  ( 9.590870124851306855, 9.322893336083156512, 27.95908392747358917 ) ) ;
#1420 = FACE_OUTER_BOUND ( 'NONE', #3483, .T. ) ;
#1421 = ORIENTED_EDGE ( 'NONE', *, *, #5944, .T. ) ;
#1422 = CARTESIAN_POINT ( 'NONE',  ( 45.92560378283280187, 36.99336990414421678, -35.00000000000000000 ) ) ;
#1423 = FACE_BOUND ( 'NONE', #4381, .T. ) ;
#1424 = CARTESIAN_POINT ( 'NONE',  ( -12.00000000000000000, 50.91502622129181788, -20.00000000000000000 ) ) ;
#1425 = ORIENTED_EDGE ( 'NONE', *, *, #2852, .F. ) ;
#1426 = CARTESIAN_POINT ( 'NONE',  ( -11.99999999999999645, 12.00000000000000355, -20.00000000000000000 ) ) ;
#1427 = CARTESIAN_POINT ( 'NONE',  ( 4.002955306052617068, -14.21240711833874037, 38.32637886702303121 ) ) ;
#1428 = ORIENTED_EDGE ( 'NONE', *, *, #561, .T. ) ;
#1429 = EDGE_LOOP ( 'NONE', ( #234, #3916, #5684, #1556 ) ) ;
#1430 = DIRECTION ( 'NONE',  ( -0.000000000000000000, -0.000000000000000000, -1.000000000000000000 ) ) ;
#1431 = LINE ( 'NONE', #5741, #4929 ) ;
#1432 = PLANE ( 'NONE',  #1356 ) ;
#1433 = DIRECTION ( 'NONE',  ( 0.07194996680737264505, 0.07194996680737218708, -0.9948097328398209926 ) ) ;
#1434 = ADVANCED_FACE ( 'NONE', ( #3546 ), #174, .F. ) ;
#1435 = FACE_OUTER_BOUND ( 'NONE', #1990, .T. ) ;
#1436 = AXIS2_PLACEMENT_3D ( 'NONE', #1048, #5416, #5246 ) ;
#1437 = ORIENTED_EDGE ( 'NONE', *, *, #531, .T. ) ;
#1438 = CARTESIAN_POINT ( 'NONE',  ( 6.737147714782516950, 13.11522978513662885, 38.26633100282688105 ) ) ;
#1439 = LINE ( 'NONE', #2975, #4855 ) ;
#1440 = CARTESIAN_POINT ( 'NONE',  ( -55.48030965892933608, -45.89047003626479437, 35.00000000000000000 ) ) ;
#1441 = MECHANICAL_DESIGN_GEOMETRIC_PRESENTATION_REPRESENTATION (  '', ( #2545 ), #5126 ) ;
#1442 = EDGE_CURVE ( 'NONE', #3100, #2065, #4052, .T. ) ;
#1443 = ORIENTED_EDGE ( 'NONE', *, *, #2208, .F. ) ;
#1444 = DIRECTION ( 'NONE',  ( 0.9880900209011910240, -0.1538769332794358846, 0.000000000000000000 ) ) ;
#1445 = CIRCLE ( 'NONE', #4942, 80.00000000000000000 ) ;
#1446 = CARTESIAN_POINT ( 'NONE',  ( -9.462636878983097688, -7.610208295502463471, 25.48187184588751464 ) ) ;
#1447 = CIRCLE ( 'NONE', #581, 80.00000000000000000 ) ;
#1448 = DIRECTION ( 'NONE',  ( 1.000000000000000000, 0.000000000000000000, 0.000000000000000000 ) ) ;
#1449 = AXIS2_PLACEMENT_3D ( 'NONE', #5779, #2505, #4363 ) ;
#1450 = EDGE_CURVE ( 'NONE', #1368, #5498, #1759, .T. ) ;
#1451 = PRODUCT_DEFINITION_CONTEXT ( 'detailed design', #5772, 'design' ) ;
#1452 = VECTOR ( 'NONE', #414, 1000.000000000000000 ) ;
#1453 = CARTESIAN_POINT ( 'NONE',  ( -10.19629538391971124, 10.19629538389110124, 35.54424335298404003 ) ) ;
#1454 = LINE ( 'NONE', #4761, #3957 ) ;
#1455 = ORIENTED_EDGE ( 'NONE', *, *, #366, .T. ) ;
#1456 = CARTESIAN_POINT ( 'NONE',  ( 68.69027832784067300, -26.57196568621440491, 35.13717928826310555 ) ) ;
#1457 = LINE ( 'NONE', #2916, #3060 ) ;
#1458 = FACE_OUTER_BOUND ( 'NONE', #2159, .T. ) ;
#1459 = ORIENTED_EDGE ( 'NONE', *, *, #5260, .T. ) ;
#1460 = DIRECTION ( 'NONE',  ( -0.4999999999999920619, -0.8660254037844431485, 0.000000000000000000 ) ) ;
#1461 = CARTESIAN_POINT ( 'NONE',  ( 9.515772848102850290, -10.27564057804868725, 33.05475024408053741 ) ) ;
#1462 = ORIENTED_EDGE ( 'NONE', *, *, #749, .F. ) ;
#1463 = ORIENTED_EDGE ( 'NONE', *, *, #2933, .F. ) ;
#1464 = DIRECTION ( 'NONE',  ( -0.000000000000000000, 0.000000000000000000, 1.000000000000000000 ) ) ;
#1465 = DIRECTION ( 'NONE',  ( -1.000000000000000000, -0.000000000000000000, -0.000000000000000000 ) ) ;
#1466 = CARTESIAN_POINT ( 'NONE',  ( -12.49999999999999822, 67.50000000000000000, -19.00000000000000711 ) ) ;
#1467 =( NAMED_UNIT ( * ) PLANE_ANGLE_UNIT ( ) SI_UNIT ( $, .RADIAN. ) );
#1468 = CIRCLE ( 'NONE', #1660, 12.49999999999999822 ) ;
#1469 = FACE_OUTER_BOUND ( 'NONE', #1389, .T. ) ;
#1470 = CARTESIAN_POINT ( 'NONE',  ( 8.999999999999998224, -8.999999999999998224, -167.0000000000000284 ) ) ;
#1471 = AXIS2_PLACEMENT_3D ( 'NONE', #1791, #5197, #4601 ) ;
#1472 = AXIS2_PLACEMENT_3D ( 'NONE', #3858, #1020, #4266 ) ;
#1473 = VERTEX_POINT ( 'NONE', #681 ) ;
#1474 = CARTESIAN_POINT ( 'NONE',  ( 1.839547822007356226, 11.79779776130985880, 30.71783115363461647 ) ) ;
#1475 = VECTOR ( 'NONE', #917, 1000.000000000000000 ) ;
#1476 = CARTESIAN_POINT ( 'NONE',  ( -3.333333333333289961, 9.999999999999998224, 23.00000000000000000 ) ) ;
#1477 = CARTESIAN_POINT ( 'NONE',  ( -10.37777353962477278, -10.37777353962696303, 38.05103295300743582 ) ) ;
#1478 = ORIENTED_EDGE ( 'NONE', *, *, #4270, .F. ) ;
#1479 = DIRECTION ( 'NONE',  ( 1.000000000000000000, 0.000000000000000000, 0.000000000000000000 ) ) ;
#1480 = AXIS2_PLACEMENT_3D ( 'NONE', #4135, #3179, #5087 ) ;
#1481 = CARTESIAN_POINT ( 'NONE',  ( -10.77711034800892875, -7.077301327650769025, 30.61076202992614270 ) ) ;
#1482 = ADVANCED_FACE ( 'NONE', ( #625 ), #2648, .F. ) ;
#1483 = EDGE_CURVE ( 'NONE', #4960, #2705, #1274, .T. ) ;
#1484 = CARTESIAN_POINT ( 'NONE',  ( 10.43169748385510687, -11.73806315776973719, 38.00000000000000000 ) ) ;
#1485 = EDGE_CURVE ( 'NONE', #149, #5582, #5139, .T. ) ;
#1486 = DIRECTION ( 'NONE',  ( -0.000000000000000000, -0.000000000000000000, -1.000000000000000000 ) ) ;
#1487 = EDGE_CURVE ( 'NONE', #4312, #1918, #393, .T. ) ;
#1488 = CARTESIAN_POINT ( 'NONE',  ( 8.930195544526858598, -11.65680117706489760, 38.09189898655662887 ) ) ;
#1489 = EDGE_LOOP ( 'NONE', ( #5089, #5421 ) ) ;
#1490 = CARTESIAN_POINT ( 'NONE',  ( 12.00000000000000000, 0.000000000000000000, -20.00000000000000000 ) ) ;
#1491 = EDGE_LOOP ( 'NONE', ( #4814, #190 ) ) ;
#1492 = FACE_BOUND ( 'NONE', #2170, .T. ) ;
#1493 = CARTESIAN_POINT ( 'NONE',  ( 6.787634061845150946, -9.554965159330784275, 25.51646427192168787 ) ) ;
#1494 = EDGE_CURVE ( 'NONE', #1644, #5747, #1575, .T. ) ;
#1495 = VERTEX_POINT ( 'NONE', #4070 ) ;
#1496 = CARTESIAN_POINT ( 'NONE',  ( -1.630640067418198669E-13, 67.50000000000002842, -35.00000000000000000 ) ) ;
#1497 = ORIENTED_EDGE ( 'NONE', *, *, #208, .T. ) ;
#1498 = CARTESIAN_POINT ( 'NONE',  ( -55.00000000000010658, 21.27605460799956205, 35.00000000000000000 ) ) ;
#1499 = DIRECTION ( 'NONE',  ( -1.000000000000000000, 0.000000000000000000, -0.000000000000000000 ) ) ;
#1500 = CARTESIAN_POINT ( 'NONE',  ( 33.70629803557132931, -9.018075675152060100, -3.469446951953614189E-15 ) ) ;
#1501 = DIRECTION ( 'NONE',  ( 1.000000000000000000, 0.000000000000000000, 0.000000000000000000 ) ) ;
#1502 = CARTESIAN_POINT ( 'NONE',  ( 11.39263409468387067, -7.228600378928579318, 33.15620577507543487 ) ) ;
#1503 = ORIENTED_EDGE ( 'NONE', *, *, #1519, .F. ) ;
#1504 = CARTESIAN_POINT ( 'NONE',  ( 3.423848683943063964, 9.833809958618568103, 25.60794474275442667 ) ) ;
#1505 = CARTESIAN_POINT ( 'NONE',  ( -0.8289898103093434889, 9.900940235153617763, 22.73823205004162773 ) ) ;
#1506 = DIRECTION ( 'NONE',  ( 0.000000000000000000, 0.000000000000000000, 1.000000000000000000 ) ) ;
#1507 = ORIENTED_EDGE ( 'NONE', *, *, #1228, .F. ) ;
#1508 = CARTESIAN_POINT ( 'NONE',  ( -52.58482424179536707, 72.37680137756343868, -40.00000000000000000 ) ) ;
#1509 = ORIENTED_EDGE ( 'NONE', *, *, #2047, .F. ) ;
#1510 = PRODUCT_DEFINITION_CONTEXT ( 'detailed design', #4404, 'design' ) ;
#1511 = EDGE_CURVE ( 'NONE', #1523, #2445, #3848, .T. ) ;
#1512 = CARTESIAN_POINT ( 'NONE',  ( -9.000000000000005329, 8.999999999988014920, 23.06137295785748265 ) ) ;
#1513 = FACE_OUTER_BOUND ( 'NONE', #4493, .T. ) ;
#1514 = ORIENTED_EDGE ( 'NONE', *, *, #4495, .F. ) ;
#1515 = LINE ( 'NONE', #2044, #2144 ) ;
#1516 = DIRECTION ( 'NONE',  ( -0.000000000000000000, 0.000000000000000000, 1.000000000000000000 ) ) ;
#1517 = CARTESIAN_POINT ( 'NONE',  ( 0.000000000000000000, 89.46264649666795776, 40.00000000000000000 ) ) ;
#1518 = ORIENTED_EDGE ( 'NONE', *, *, #946, .F. ) ;
#1519 = EDGE_CURVE ( 'NONE', #3265, #3338, #3744, .T. ) ;
#1520 = DIRECTION ( 'NONE',  ( -0.07194996680737253403, -0.07194996680737229811, -0.9948097328398209926 ) ) ;
#1521 = CARTESIAN_POINT ( 'NONE',  ( 6.652779355836718977, -8.964415603276487232, 22.96342386064222296 ) ) ;
#1522 = ORIENTED_EDGE ( 'NONE', *, *, #2701, .T. ) ;
#1523 = VERTEX_POINT ( 'NONE', #2766 ) ;
#1524 = CARTESIAN_POINT ( 'NONE',  ( 14.67638808697554964, -1.485455082520059617E-11, 38.18288438803429585 ) ) ;
#1525 = DIRECTION ( 'NONE',  ( -0.000000000000000000, 0.000000000000000000, -1.000000000000000000 ) ) ;
#1526 = DIRECTION ( 'NONE',  ( 0.000000000000000000, 0.000000000000000000, 1.000000000000000000 ) ) ;
#1527 = DIRECTION ( 'NONE',  ( 0.000000000000000000, 0.000000000000000000, 1.000000000000000000 ) ) ;
#1528 = ADVANCED_FACE ( 'NONE', ( #2679 ), #2706, .T. ) ;
#1529 = DIRECTION ( 'NONE',  ( 0.000000000000000000, 0.000000000000000000, -1.000000000000000000 ) ) ;
#1530 = ORIENTED_EDGE ( 'NONE', *, *, #2087, .T. ) ;
#1531 = ORIENTED_EDGE ( 'NONE', *, *, #1373, .T. ) ;
#1532 = CARTESIAN_POINT ( 'NONE',  ( 2.035630462091352122, 14.63234267792704557, 38.34842398122203377 ) ) ;
#1533 = CARTESIAN_POINT ( 'NONE',  ( 9.969668718019493170, 9.144590365090015993, 22.73823205004162418 ) ) ;
#1534 = DIRECTION ( 'NONE',  ( 1.000000000000000000, 0.000000000000000000, 0.000000000000000000 ) ) ;
#1535 = AXIS2_PLACEMENT_3D ( 'NONE', #218, #2089, #5028 ) ;
#1536 = ORIENTED_EDGE ( 'NONE', *, *, #3030, .T. ) ;
#1537 = DIRECTION ( 'NONE',  ( 1.224646799147353207E-16, 1.000000000000000000, 0.000000000000000000 ) ) ;
#1538 = CARTESIAN_POINT ( 'NONE',  ( -10.46302782743270754, -5.247549479766034253, 28.11481907968152782 ) ) ;
#1539 = VECTOR ( 'NONE', #3565, 1000.000000000000000 ) ;
#1540 = ORIENTED_EDGE ( 'NONE', *, *, #3786, .T. ) ;
#1541 = VECTOR ( 'NONE', #6048, 1000.000000000000000 ) ;
#1542 = CARTESIAN_POINT ( 'NONE',  ( -9.981067540164714202, -9.981067540164714202, 22.73823205004162773 ) ) ;
#1543 = TOROIDAL_SURFACE ( 'NONE', #5037, 72.00000000000004263, 10.00000000000000000 ) ;
#1544 = AXIS2_PLACEMENT_3D ( 'NONE', #4593, #4712, #907 ) ;
#1545 = CARTESIAN_POINT ( 'NONE',  ( 11.39256393965315439, 7.228764404800521959, 33.15620429642044797 ) ) ;
#1546 = DIRECTION ( 'NONE',  ( 0.7787725926866081450, 0.6273063437270328668, 0.000000000000000000 ) ) ;
#1547 = CIRCLE ( 'NONE', #3933, 99.00000000000000000 ) ;
#1548 = VERTEX_POINT ( 'NONE', #2265 ) ;
#1549 = DIRECTION ( 'NONE',  ( 0.9326495259660518844, -0.3607836771741464998, 0.000000000000000000 ) ) ;
#1550 = FILL_AREA_STYLE_COLOUR ( '', #1627 ) ;
#1551 = DIRECTION ( 'NONE',  ( 0.000000000000000000, 0.000000000000000000, 1.000000000000000000 ) ) ;
#1552 = AXIS2_PLACEMENT_3D ( 'NONE', #1924, #493, #5281 ) ;
#1553 = CARTESIAN_POINT ( 'NONE',  ( 8.785602912694960409, -10.67327843797380815, 33.09221060678261495 ) ) ;
#1554 = COLOUR_RGB ( '',0.7921568627450980005, 0.8196078431372548767, 0.9333333333333333481 ) ;
#1555 = ORIENTED_EDGE ( 'NONE', *, *, #3795, .F. ) ;
#1556 = ORIENTED_EDGE ( 'NONE', *, *, #4137, .F. ) ;
#1557 = DIRECTION ( 'NONE',  ( 0.000000000000000000, 0.000000000000000000, 1.000000000000000000 ) ) ;
#1558 = EDGE_CURVE ( 'NONE', #6127, #4523, #4469, .T. ) ;
#1559 = ADVANCED_FACE ( 'NONE', ( #1303 ), #3663, .F. ) ;
#1560 = CARTESIAN_POINT ( 'NONE',  ( 4.999999999999380940, -89.46264649666795776, -40.00000000000000000 ) ) ;
#1561 = DIRECTION ( 'NONE',  ( -0.000000000000000000, 0.000000000000000000, 1.000000000000000000 ) ) ;
#1562 = CARTESIAN_POINT ( 'NONE',  ( 1.131281550719567528E-13, 1.761763928569687004E-14, -35.00000000000000000 ) ) ;
#1563 = VECTOR ( 'NONE', #5339, 1000.000000000000227 ) ;
#1564 = ORIENTED_EDGE ( 'NONE', *, *, #409, .T. ) ;
#1565 = ADVANCED_FACE ( 'NONE', ( #5516 ), #329, .T. ) ;
#1566 = DIRECTION ( 'NONE',  ( 0.000000000000000000, 0.000000000000000000, 1.000000000000000000 ) ) ;
#1567 = CARTESIAN_POINT ( 'NONE',  ( 9.902916272933978803, -1.657983872361911803, 22.73823205004162418 ) ) ;
#1568 = CARTESIAN_POINT ( 'NONE',  ( -10.72018218391586686, -10.03536489533594889, 38.06196296973735826 ) ) ;
#1569 = ORIENTED_EDGE ( 'NONE', *, *, #4331, .F. ) ;
#1570 = DIRECTION ( 'NONE',  ( -0.000000000000000000, -0.000000000000000000, 1.000000000000000000 ) ) ;
#1571 = VECTOR ( 'NONE', #5524, 1000.000000000000000 ) ;
#1572 = CARTESIAN_POINT ( 'NONE',  ( -9.928243323025453648, -0.8581648076836896344, 25.63579099555280294 ) ) ;
#1573 = CIRCLE ( 'NONE', #5462, 80.00000000000000000 ) ;
#1574 = ORIENTED_EDGE ( 'NONE', *, *, #1415, .T. ) ;
#1575 = CIRCLE ( 'NONE', #3357, 9.500000000000005329 ) ;
#1576 = CARTESIAN_POINT ( 'NONE',  ( -11.08488032081242558, -11.08488032081241847, 38.00000000000000000 ) ) ;
#1577 = VECTOR ( 'NONE', #214, 999.9999999999998863 ) ;
#1578 = CARTESIAN_POINT ( 'NONE',  ( 14.63232105816060624, 2.035738251814317223, 38.34842656511671066 ) ) ;
#1579 = CYLINDRICAL_SURFACE ( 'NONE', #2668, 12.49999999999999822 ) ;
#1580 = VECTOR ( 'NONE', #1520, 1000.000000000000000 ) ;
#1581 = ORIENTED_EDGE ( 'NONE', *, *, #3578, .F. ) ;
#1582 = CYLINDRICAL_SURFACE ( 'NONE', #5938, 12.50000000000139089 ) ;
#1583 = FACE_OUTER_BOUND ( 'NONE', #278, .T. ) ;
#1584 = CARTESIAN_POINT ( 'NONE',  ( -3.570559693971999302E-14, -10.89081796499577237, 28.17941898721254290 ) ) ;
#1585 = EDGE_LOOP ( 'NONE', ( #5295, #2692, #771, #3509 ) ) ;
#1586 = DIRECTION ( 'NONE',  ( -0.000000000000000000, -0.000000000000000000, -1.000000000000000000 ) ) ;
#1587 = EDGE_LOOP ( 'NONE', ( #2607, #2798, #246, #206 ) ) ;
#1588 = DIRECTION ( 'NONE',  ( 8.673617379884026597E-16, -1.000000000000000000, 0.000000000000000000 ) ) ;
#1589 = DIRECTION ( 'NONE',  ( -0.5000000000000037748, 0.8660254037844365982, 0.000000000000000000 ) ) ;
#1590 = CARTESIAN_POINT ( 'NONE',  ( 7.182140071210238271E-14, -8.916303653273167033E-14, -35.00000000000000000 ) ) ;
#1591 = CARTESIAN_POINT ( 'NONE',  ( -11.08488032081242380, -11.08488032081242025, 38.00000000000000000 ) ) ;
#1592 = EDGE_CURVE ( 'NONE', #3297, #2393, #4603, .T. ) ;
#1593 = EDGE_CURVE ( 'NONE', #5503, #719, #355, .T. ) ;
#1594 = VERTEX_POINT ( 'NONE', #1328 ) ;
#1595 = CARTESIAN_POINT ( 'NONE',  ( 8.662453428863081228, 10.23348454756166070, 30.54531259719474079 ) ) ;
#1596 = CARTESIAN_POINT ( 'NONE',  ( 9.999999999999998224, -5.833333333333365900, 23.00000000000000000 ) ) ;
#1597 = ORIENTED_EDGE ( 'NONE', *, *, #5103, .F. ) ;
#1598 = CARTESIAN_POINT ( 'NONE',  ( 54.99999999999999289, 6.349087922075113966E-13, -35.00000000000000000 ) ) ;
#1599 = ADVANCED_FACE ( 'NONE', ( #3231 ), #299, .T. ) ;
#1600 = CARTESIAN_POINT ( 'NONE',  ( -10.89081796499577059, -0.8880320553140184092, 28.17941898721253580 ) ) ;
#1601 = ORIENTED_EDGE ( 'NONE', *, *, #2522, .T. ) ;
#1602 = PLANE ( 'NONE',  #5833 ) ;
#1603 = EDGE_CURVE ( 'NONE', #1883, #2239, #4416, .T. ) ;
#1604 = CARTESIAN_POINT ( 'NONE',  ( 11.71459457793454639, 6.400384853991321954, 33.18278774224378225 ) ) ;
#1605 = DIRECTION ( 'NONE',  ( 0.000000000000000000, -0.000000000000000000, -1.000000000000000000 ) ) ;
#1606 = VERTEX_POINT ( 'NONE', #6072 ) ;
#1607 = DIRECTION ( 'NONE',  ( -0.5000000000000001110, -0.8660254037844385966, 0.000000000000000000 ) ) ;
#1608 = CARTESIAN_POINT ( 'NONE',  ( -0.9193131588476529670, -11.85339260696609465, 30.72304697887226865 ) ) ;
#1609 = ORIENTED_EDGE ( 'NONE', *, *, #1039, .F. ) ;
#1610 = CARTESIAN_POINT ( 'NONE',  ( 68.69027832783777399, 26.57196568621521138, 35.13717928826270054 ) ) ;
#1611 = VERTEX_POINT ( 'NONE', #1793 ) ;
#1612 = LINE ( 'NONE', #5837, #97 ) ;
#1613 = CARTESIAN_POINT ( 'NONE',  ( -74.61196207728391983, 28.86269417393235415, 35.00000000000000000 ) ) ;
#1614 = APPLICATION_PROTOCOL_DEFINITION ( 'draft international standard', 'automotive_design', 1998, #5973 ) ;
#1615 = CARTESIAN_POINT ( 'NONE',  ( -68.69027832783800136, -26.57196568621473531, 35.13717928826270054 ) ) ;
#1616 = CARTESIAN_POINT ( 'NONE',  ( 55.71784976887228424, -21.55374571496028224, 35.00000000000000000 ) ) ;
#1617 = ORIENTED_EDGE ( 'NONE', *, *, #5715, .T. ) ;
#1618 = CARTESIAN_POINT ( 'NONE',  ( 10.19494410001831142, 9.858401829237472214, 33.01259202755186095 ) ) ;
#1619 = CARTESIAN_POINT ( 'NONE',  ( 9.999999999999998224, 1.666666666666619223, 23.00000000000000000 ) ) ;
#1620 = CARTESIAN_POINT ( 'NONE',  ( -5.141101056459331353, 67.50000000000000000, 19.00000000000000000 ) ) ;
#1621 = ORIENTED_EDGE ( 'NONE', *, *, #856, .F. ) ;
#1622 = CARTESIAN_POINT ( 'NONE',  ( -10.89081796499577059, 0.8880320553140812478, 28.17941898721253580 ) ) ;
#1623 = EDGE_LOOP ( 'NONE', ( #3718, #5012, #796, #422 ) ) ;
#1624 = LINE ( 'NONE', #1689, #3327 ) ;
#1625 = EDGE_CURVE ( 'NONE', #3297, #15, #5041, .T. ) ;
#1626 = CIRCLE ( 'NONE', #1064, 80.00000000000000000 ) ;
#1627 = COLOUR_RGB ( '',0.7921568627450980005, 0.8196078431372548767, 0.9333333333333333481 ) ;
#1628 = CARTESIAN_POINT ( 'NONE',  ( 12.01612071878465571, 7.393143600131257820, 35.69844150329612376 ) ) ;
#1629 = EDGE_CURVE ( 'NONE', #354, #1672, #6, .T. ) ;
#1630 = CARTESIAN_POINT ( 'NONE',  ( 85.08403291566575888, -27.64547812922912939, 40.00000000000000000 ) ) ;
#1631 = ORIENTED_EDGE ( 'NONE', *, *, #1930, .T. ) ;
#1632 = CARTESIAN_POINT ( 'NONE',  ( -3.000397777471226934, 9.000000000000003553, 23.18288458324517975 ) ) ;
#1633 = EDGE_CURVE ( 'NONE', #2290, #1920, #3384, .T. ) ;
#1634 = AXIS2_PLACEMENT_3D ( 'NONE', #4660, #5720, #1448 ) ;
#1635 = DIRECTION ( 'NONE',  ( 0.1538769332794359679, 0.9880900209011910240, 0.000000000000000000 ) ) ;
#1636 = CARTESIAN_POINT ( 'NONE',  ( 0.9833031778629115482, -13.77854189090673742, 35.81030296219173437 ) ) ;
#1637 = CIRCLE ( 'NONE', #276, 100.0000000000000000 ) ;
#1638 = ORIENTED_EDGE ( 'NONE', *, *, #3009, .F. ) ;
#1639 = CYLINDRICAL_SURFACE ( 'NONE', #6037, 14.67638808697554964 ) ;
#1640 = ORIENTED_EDGE ( 'NONE', *, *, #4260, .T. ) ;
#1641 = CARTESIAN_POINT ( 'NONE',  ( 12.74784844746000445, 7.336363311096732787, 38.12594328983447411 ) ) ;
#1642 = CARTESIAN_POINT ( 'NONE',  ( 27.60043906316099083, 27.60043906316109386, 35.00000000000000000 ) ) ;
#1643 = SHAPE_DEFINITION_REPRESENTATION ( #6034, #4716 ) ;
#1644 = VERTEX_POINT ( 'NONE', #2658 ) ;
#1645 = CARTESIAN_POINT ( 'NONE',  ( 62.30180741492871022, 50.18450749816254586, 35.00000000000000000 ) ) ;
#1646 = DIRECTION ( 'NONE',  ( -0.000000000000000000, -0.000000000000000000, 1.000000000000000000 ) ) ;
#1647 = ORIENTED_EDGE ( 'NONE', *, *, #1592, .F. ) ;
#1648 = TOROIDAL_SURFACE ( 'NONE', #1080, 72.00000000000004263, 10.00000000000000000 ) ;
#1649 = VERTEX_POINT ( 'NONE', #544 ) ;
#1650 = CARTESIAN_POINT ( 'NONE',  ( 47.58482424179642578, 72.37680137756268550, -40.00000000000000000 ) ) ;
#1651 = CARTESIAN_POINT ( 'NONE',  ( -12.00000000000000000, 0.000000000000000000, -20.00000000000000000 ) ) ;
#1652 = CARTESIAN_POINT ( 'NONE',  ( -58.45671475544979501, 33.74999999999974420, 35.00000000000000000 ) ) ;
#1653 = CLOSED_SHELL ( 'NONE', ( #3387, #2095, #2312, #292, #4074, #4285, #1565, #5408, #3225, #5043, #1122, #5390 ) ) ;
#1654 = VERTEX_POINT ( 'NONE', #1037 ) ;
#1655 = DIRECTION ( 'NONE',  ( -0.3607836771741652626, 0.9326495259660446679, 0.000000000000000000 ) ) ;
#1656 = VECTOR ( 'NONE', #4326, 1000.000000000000000 ) ;
#1657 = CARTESIAN_POINT ( 'NONE',  ( -8.965668681055127820, -0.8304760625348956982, 23.09216300389307719 ) ) ;
#1658 = ORIENTED_EDGE ( 'NONE', *, *, #5791, .T. ) ;
#1659 = CARTESIAN_POINT ( 'NONE',  ( 0.000000000000000000, 0.000000000000000000, 38.99999999999995737 ) ) ;
#1660 = AXIS2_PLACEMENT_3D ( 'NONE', #3177, #3716, #2680 ) ;
#1661 = AXIS2_PLACEMENT_3D ( 'NONE', #4698, #3299, #5581 ) ;
#1662 = EDGE_CURVE ( 'NONE', #4523, #816, #3531, .T. ) ;
#1663 = EDGE_CURVE ( 'NONE', #993, #5773, #1951, .T. ) ;
#1664 = CIRCLE ( 'NONE', #1183, 72.00000000000004263 ) ;
#1665 = CARTESIAN_POINT ( 'NONE',  ( 9.999999999999998224, 9.999999999999998224, -20.00000000000000000 ) ) ;
#1666 = ORIENTED_EDGE ( 'NONE', *, *, #2629, .F. ) ;
#1667 = CARTESIAN_POINT ( 'NONE',  ( -9.981067540164714202, 9.981067540164714202, 22.73823205004162418 ) ) ;
#1668 = AXIS2_PLACEMENT_3D ( 'NONE', #4807, #953, #2875 ) ;
#1669 = EDGE_CURVE ( 'NONE', #5346, #4900, #67, .T. ) ;
#1670 = AXIS2_PLACEMENT_3D ( 'NONE', #654, #3955, #4880 ) ;
#1671 = CARTESIAN_POINT ( 'NONE',  ( -3.019346778933469366, -14.42236408824967775, 38.33740271606986738 ) ) ;
#1672 = VERTEX_POINT ( 'NONE', #416 ) ;
#1673 = LINE ( 'NONE', #2079, #587 ) ;
#1674 = ORIENTED_EDGE ( 'NONE', *, *, #5649, .T. ) ;
#1675 = CARTESIAN_POINT ( 'NONE',  ( 8.586443133426902668E-15, -8.586443133426886890E-15, 20.00000000000000000 ) ) ;
#1676 = CARTESIAN_POINT ( 'NONE',  ( 12.31015466235495026, 79.04720167209526949, 35.00000000000000000 ) ) ;
#1677 = APPLICATION_PROTOCOL_DEFINITION ( 'draft international standard', 'automotive_design', 1998, #5891 ) ;
#1678 = CARTESIAN_POINT ( 'NONE',  ( 62.30180741492925733, -50.18450749816190637, -35.00000000000000711 ) ) ;
#1679 = DIRECTION ( 'NONE',  ( -0.5000000000000042188, 0.8660254037844362651, 0.000000000000000000 ) ) ;
#1680 = EDGE_CURVE ( 'NONE', #1401, #5045, #2859, .T. ) ;
#1681 = VERTEX_POINT ( 'NONE', #5199 ) ;
#1682 = CARTESIAN_POINT ( 'NONE',  ( 6.787591074359449195, 9.554964866038103466, 25.51646829178083564 ) ) ;
#1683 = CARTESIAN_POINT ( 'NONE',  ( 9.939337621248920840, 6.642184745761413822, 22.73823205004162418 ) ) ;
#1684 = DIRECTION ( 'NONE',  ( 0.000000000000000000, 0.000000000000000000, 1.000000000000000000 ) ) ;
#1685 = ORIENTED_EDGE ( 'NONE', *, *, #3910, .T. ) ;
#1686 = CARTESIAN_POINT ( 'NONE',  ( 15.00000000000000000, 50.91502622129181788, 35.00000000000000000 ) ) ;
#1687 = CARTESIAN_POINT ( 'NONE',  ( -10.59950146047779640, 4.399209358691972049, 28.13666863833445220 ) ) ;
#1688 = EDGE_LOOP ( 'NONE', ( #3440, #2097, #3588, #3386 ) ) ;
#1689 = CARTESIAN_POINT ( 'NONE',  ( -57.58482424179695869, -72.37680137756228760, -79.99999999999998579 ) ) ;
#1690 = CARTESIAN_POINT ( 'NONE',  ( 11.60016251788559849, 72.19966265504864111, 35.04915833130703362 ) ) ;
#1691 = DIRECTION ( 'NONE',  ( 0.000000000000000000, -1.000000000000000000, 0.000000000000000000 ) ) ;
#1692 = FACE_OUTER_BOUND ( 'NONE', #4176, .T. ) ;
#1693 = CARTESIAN_POINT ( 'NONE',  ( -5.809855716632613465, 9.930636381741159369, 22.73823205004162418 ) ) ;
#1694 = EDGE_CURVE ( 'NONE', #2123, #3856, #3625, .T. ) ;
#1695 = LINE ( 'NONE', #3172, #5157 ) ;
#1696 = ORIENTED_EDGE ( 'NONE', *, *, #127, .T. ) ;
#1697 = CARTESIAN_POINT ( 'NONE',  ( -8.999999999999992895, -3.000397777471252692, 23.18288458324513357 ) ) ;
#1698 = VERTEX_POINT ( 'NONE', #6130 ) ;
#1699 = CARTESIAN_POINT ( 'NONE',  ( 27.50000000000043698, -47.63139720814386635, 35.00000000000000000 ) ) ;
#1700 = LINE ( 'NONE', #3142, #293 ) ;
#1701 = ADVANCED_FACE ( 'NONE', ( #4693 ), #2824, .F. ) ;
#1702 = DIRECTION ( 'NONE',  ( 0.000000000000000000, 0.000000000000000000, 1.000000000000000000 ) ) ;
#1703 = DIRECTION ( 'NONE',  ( 0.000000000000000000, 0.000000000000000000, 1.000000000000000000 ) ) ;
#1704 = EDGE_LOOP ( 'NONE', ( #4055, #1172, #2244, #434 ) ) ;
#1705 = CARTESIAN_POINT ( 'NONE',  ( -11.33314185116958051, 72.77350886804100583, 35.13717928826310555 ) ) ;
#1706 = LINE ( 'NONE', #5609, #2127 ) ;
#1707 = CARTESIAN_POINT ( 'NONE',  ( -5.161660887237596640, 13.74708875321003809, 38.15586426248332685 ) ) ;
#1708 = CARTESIAN_POINT ( 'NONE',  ( 0.000000000000000000, 0.000000000000000000, -40.00000000000000000 ) ) ;
#1709 = ADVANCED_FACE ( 'NONE', ( #6098 ), #5632, .F. ) ;
#1710 = ORIENTED_EDGE ( 'NONE', *, *, #513, .F. ) ;
#1711 = CARTESIAN_POINT ( 'NONE',  ( 12.74242197681752664, -1.902388932222474294, 33.26151580524049933 ) ) ;
#1712 = CARTESIAN_POINT ( 'NONE',  ( -10.27564057804868725, 9.515772848102853843, 33.05475024408053031 ) ) ;
#1713 = VERTEX_POINT ( 'NONE', #1422 ) ;
#1714 = FACE_OUTER_BOUND ( 'NONE', #661, .T. ) ;
#1715 = LINE ( 'NONE', #2497, #3224 ) ;
#1716 = CARTESIAN_POINT ( 'NONE',  ( -1.131281550719566266E-13, -1.761763928569765259E-14, 35.00000000000000000 ) ) ;
#1717 = DIRECTION ( 'NONE',  ( -0.000000000000000000, 0.000000000000000000, -1.000000000000000000 ) ) ;
#1718 = CARTESIAN_POINT ( 'NONE',  ( -10.43169748385510509, 11.73806315776973719, 38.00000000000000000 ) ) ;
#1719 = AXIS2_PLACEMENT_3D ( 'NONE', #1630, #2639, #5452 ) ;
#1720 = CARTESIAN_POINT ( 'NONE',  ( -10.04707028972858929, -9.166555234036120936, 25.36260747786040426 ) ) ;
#1721 = ORIENTED_EDGE ( 'NONE', *, *, #2318, .T. ) ;
#1722 = DIRECTION ( 'NONE',  ( 1.000000000000000000, 0.000000000000000000, 0.000000000000000000 ) ) ;
#1723 = VECTOR ( 'NONE', #252, 1000.000000000000000 ) ;
#1724 = ORIENTED_EDGE ( 'NONE', *, *, #4091, .F. ) ;
#1725 =( REPRESENTATION_RELATIONSHIP ('NONE','NONE', #4716, #2176 ) REPRESENTATION_RELATIONSHIP_WITH_TRANSFORMATION ( #3691 )SHAPE_REPRESENTATION_RELATIONSHIP( ) );
#1726 = DIRECTION ( 'NONE',  ( 0.000000000000000000, 0.000000000000000000, 1.000000000000000000 ) ) ;
#1727 = MECHANICAL_DESIGN_GEOMETRIC_PRESENTATION_REPRESENTATION (  '', ( #59 ), #1245 ) ;
#1728 = LINE ( 'NONE', #3664, #1097 ) ;
#1729 = ITEM_DEFINED_TRANSFORMATION ( 'NONE', 'NONE', #2147,  #73 ) ;
#1730 = AXIS2_PLACEMENT_3D ( 'NONE', #4764, #3779, #1817 ) ;
#1731 = CARTESIAN_POINT ( 'NONE',  ( 9.999999999999998224, -9.999999999999998224, 23.00000000000000000 ) ) ;
#1732 = CARTESIAN_POINT ( 'NONE',  ( -11.08488032081241670, 11.08488032081242558, 38.00000000000000000 ) ) ;
#1733 = CIRCLE ( 'NONE', #1833, 99.00000000000005684 ) ;
#1734 = AXIS2_PLACEMENT_3D ( 'NONE', #1317, #585, #3705 ) ;
#1735 = CARTESIAN_POINT ( 'NONE',  ( -57.35713647667095927, -46.20154318182582642, 35.00000000000000000 ) ) ;
#1736 = EDGE_CURVE ( 'NONE', #3734, #4976, #3621, .T. ) ;
#1737 = EDGE_CURVE ( 'NONE', #4211, #3523, #3332, .T. ) ;
#1738 = ORIENTED_EDGE ( 'NONE', *, *, #4727, .F. ) ;
#1739 = CARTESIAN_POINT ( 'NONE',  ( 0.000000000000000000, 67.50000000000000000, 19.00000000000000000 ) ) ;
#1740 = DIRECTION ( 'NONE',  ( 8.673617379884026597E-16, 1.000000000000000000, 0.000000000000000000 ) ) ;
#1741 = B_SPLINE_SURFACE_WITH_KNOTS ( 'NONE', 3, 1, ( 
 ( #929, #4707, #1667 ),
 ( #1718, #3623, #3567 ),
 ( #4064, #5511, #5485 ),
 ( #5981, #1214, #3105 ),
 ( #2641, #4536, #1693 ),
 ( #2511, #4399, #4748 ),
 ( #4336, #1476, #996 ),
 ( #3798, #3373, #1028 ),
 ( #1057, #26, #1505 ),
 ( #2843, #502, #4782 ),
 ( #147, #3341, #4885 ),
 ( #2383, #2907, #2937 ),
 ( #5254, #4849, #2413 ),
 ( #633, #2879, #5712 ),
 ( #5286, #4275, #535 ),
 ( #4811, #5784, #2028 ),
 ( #2001, #4302, #5749 ),
 ( #51, #1903, #3435 ) ),
 .UNSPECIFIED., .F., .F., .F.,
 ( 4, 2, 2, 2, 2, 2, 2, 2, 4 ),
 ( 2, 1, 2 ),
 ( 0.000000000000000000, 0.1250000000000000000, 0.2500000000000000000, 0.3750000000000000000, 0.5000000000000000000, 0.6250000000000000000, 0.7500000000000000000, 0.8750000000000000000, 1.000000000000000000 ),
 ( 0.000000000000000000, 1.000000000000000000, 1.017451196663891722 ),
 .UNSPECIFIED. ) ;
#1742 = DIRECTION ( 'NONE',  ( -0.9326495259660447790, -0.3607836771741651516, 0.000000000000000000 ) ) ;
#1743 = VECTOR ( 'NONE', #651, 1000.000000000000000 ) ;
#1744 =( NAMED_UNIT ( * ) SI_UNIT ( $, .STERADIAN. ) SOLID_ANGLE_UNIT ( ) );
#1745 = VECTOR ( 'NONE', #1586, 1000.000000000000000 ) ;
#1746 = CARTESIAN_POINT ( 'NONE',  ( 14.74111653287706147, -1.016991241531516321, 38.35393095385146012 ) ) ;
#1747 =( GEOMETRIC_REPRESENTATION_CONTEXT ( 3 ) GLOBAL_UNCERTAINTY_ASSIGNED_CONTEXT ( ( #1880 ) ) GLOBAL_UNIT_ASSIGNED_CONTEXT ( ( #923, #397, #5586 ) ) REPRESENTATION_CONTEXT ( 'NONE', 'WORKASPACE' ) );
#1748 = EDGE_CURVE ( 'NONE', #2101, #5574, #4607, .T. ) ;
#1749 = CARTESIAN_POINT ( 'NONE',  ( -12.01622299351614309, 7.392961014695935695, 35.69843844696172397 ) ) ;
#1750 = ORIENTED_EDGE ( 'NONE', *, *, #3047, .F. ) ;
#1751 = AXIS2_PLACEMENT_3D ( 'NONE', #428, #4197, #1164 ) ;
#1752 = CARTESIAN_POINT ( 'NONE',  ( -3.019346778933468478, 14.42236408824967420, 38.33740271606986738 ) ) ;
#1753 = CARTESIAN_POINT ( 'NONE',  ( -11.82353433160363387, -71.60642589802917257, 35.00000000000000000 ) ) ;
#1754 = LINE ( 'NONE', #5568, #3336 ) ;
#1755 = CLOSED_SHELL ( 'NONE', ( #903, #4378, #5152, #5023, #3116, #2355, #1040, #8, #56, #3308, #5561, #716, #3389, #3785, #6031, #779, #1221, #4832, #3079, #2136, #2856, #2241 ) ) ;
#1756 = DIRECTION ( 'NONE',  ( 1.000000000000000000, 0.000000000000000000, 0.000000000000000000 ) ) ;
#1757 = VECTOR ( 'NONE', #2460, 1000.000000000000000 ) ;
#1758 = DIRECTION ( 'NONE',  ( -0.000000000000000000, -0.000000000000000000, -1.000000000000000000 ) ) ;
#1759 = CIRCLE ( 'NONE', #3464, 4.999999999999990230 ) ;
#1760 = DIRECTION ( 'NONE',  ( -0.000000000000000000, 0.000000000000000000, 1.000000000000000000 ) ) ;
#1761 = EDGE_LOOP ( 'NONE', ( #3456, #1518, #756, #1564 ) ) ;
#1762 = DIRECTION ( 'NONE',  ( 1.000000000000000000, 0.000000000000000000, 0.000000000000000000 ) ) ;
#1763 = VECTOR ( 'NONE', #3197, 1000.000000000000000 ) ;
#1764 = ORIENTED_EDGE ( 'NONE', *, *, #4341, .F. ) ;
#1765 = CARTESIAN_POINT ( 'NONE',  ( 0.000000000000000000, 0.000000000000000000, 40.00000000000000000 ) ) ;
#1766 = ADVANCED_FACE ( 'NONE', ( #1359 ), #5344, .T. ) ;
#1767 = FACE_OUTER_BOUND ( 'NONE', #362, .T. ) ;
#1768 = CONTEXT_DEPENDENT_SHAPE_REPRESENTATION ( #3526, #5721 ) ;
#1769 = CARTESIAN_POINT ( 'NONE',  ( -55.48030965893044453, 45.89047003626346566, 35.00000000000000000 ) ) ;
#1770 = CARTESIAN_POINT ( 'NONE',  ( -9.999999999999998224, 9.166666666666673180, 23.00000000000000000 ) ) ;
#1771 = AXIS2_PLACEMENT_3D ( 'NONE', #3206, #12, #916 ) ;
#1772 = CARTESIAN_POINT ( 'NONE',  ( 9.557272410707515320, -9.557272410707506438, 28.03893107092314452 ) ) ;
#1773 = EDGE_LOOP ( 'NONE', ( #761, #3241, #2703, #1540, #624, #6019 ) ) ;
#1774 = CARTESIAN_POINT ( 'NONE',  ( -11.82353433160510470, 71.60642589802979785, 35.00000000000000000 ) ) ;
#1775 = DIRECTION ( 'NONE',  ( -0.4999999999999920619, -0.8660254037844431485, 0.000000000000000000 ) ) ;
#1776 = CARTESIAN_POINT ( 'NONE',  ( 10.37777353962571425, 10.37777353962603044, 38.05103295300744293 ) ) ;
#1777 = EDGE_CURVE ( 'NONE', #1918, #4090, #4897, .T. ) ;
#1778 = CARTESIAN_POINT ( 'NONE',  ( 12.45811160333930623, -3.759380242563083119, 33.24069127598784235 ) ) ;
#1779 = B_SPLINE_CURVE_WITH_KNOTS ( 'NONE', 3,
 ( #1705, #2685, #1774, #3606 ),
 .UNSPECIFIED., .F., .F.,
 ( 4, 4 ),
 ( 1.430489624538199204E-17, 0.001907370850886582142 ),
 .UNSPECIFIED. ) ;
#1780 = CARTESIAN_POINT ( 'NONE',  ( -11.02055295301484428, 6.248212340465905790, 30.63787875916901626 ) ) ;
#1781 = ORIENTED_EDGE ( 'NONE', *, *, #2108, .T. ) ;
#1782 = CARTESIAN_POINT ( 'NONE',  ( -4.002955306052619733, 14.21240711833874037, 38.32637886702303121 ) ) ;
#1783 = DIRECTION ( 'NONE',  ( 0.7787725926866162496, -0.6273063437270228748, 0.000000000000000000 ) ) ;
#1784 = ADVANCED_FACE ( 'NONE', ( #159 ), #1582, .F. ) ;
#1785 = DIRECTION ( 'NONE',  ( 1.000000000000000000, 0.000000000000000000, 0.000000000000000000 ) ) ;
#1786 = LINE ( 'NONE', #3681, #4033 ) ;
#1787 = DIRECTION ( 'NONE',  ( 1.000000000000000000, 0.000000000000000000, 0.000000000000000000 ) ) ;
#1788 = EDGE_CURVE ( 'NONE', #3906, #3800, #3130, .T. ) ;
#1789 = CARTESIAN_POINT ( 'NONE',  ( -6.563799387313615341, -12.41448144607147874, 35.72511331161845050 ) ) ;
#1790 = ORIENTED_EDGE ( 'NONE', *, *, #5419, .F. ) ;
#1791 = CARTESIAN_POINT ( 'NONE',  ( -7.182140071210238271E-14, 8.916303653273167033E-14, 35.00000000000000000 ) ) ;
#1792 = ORIENTED_EDGE ( 'NONE', *, *, #1318, .T. ) ;
#1793 = CARTESIAN_POINT ( 'NONE',  ( 8.999999999988068211, 9.000000000000005329, 23.06137295785747554 ) ) ;
#1794 = CARTESIAN_POINT ( 'NONE',  ( 58.45671475544962448, 33.75000000000001421, -35.00000000000000000 ) ) ;
#1795 = FACE_OUTER_BOUND ( 'NONE', #1587, .T. ) ;
#1796 = CARTESIAN_POINT ( 'NONE',  ( -9.999999999999998224, 0.8333333333333826642, 23.00000000000000000 ) ) ;
#1797 = DIRECTION ( 'NONE',  ( 0.000000000000000000, -1.000000000000000000, -0.000000000000000000 ) ) ;
#1798 = VERTEX_POINT ( 'NONE', #1109 ) ;
#1799 = LINE ( 'NONE', #2212, #4144 ) ;
#1800 = LINE ( 'NONE', #896, #1152 ) ;
#1801 = DIRECTION ( 'NONE',  ( -0.000000000000000000, -0.000000000000000000, -1.000000000000000000 ) ) ;
#1802 =( LENGTH_UNIT ( ) NAMED_UNIT ( * ) SI_UNIT ( .MILLI., .METRE. ) );
#1803 = CARTESIAN_POINT ( 'NONE',  ( 9.833809958618568103, -3.423848683943063964, 25.60794474275442667 ) ) ;
#1804 = CARTESIAN_POINT ( 'NONE',  ( -8.056095891487838412E-14, 1.254589464284425060E-14, -35.00000000000000000 ) ) ;
#1805 = ORIENTED_EDGE ( 'NONE', *, *, #2673, .T. ) ;
#1806 = CARTESIAN_POINT ( 'NONE',  ( -3.531709963121634210, 10.70751606408959411, 28.15279306126448233 ) ) ;
#1807 = CARTESIAN_POINT ( 'NONE',  ( -11.60016251788559849, -72.19966265504864111, 35.04915833130703362 ) ) ;
#1808 = EDGE_LOOP ( 'NONE', ( #630, #3406 ) ) ;
#1809 = FACE_OUTER_BOUND ( 'NONE', #145, .T. ) ;
#1810 = EDGE_CURVE ( 'NONE', #103, #5851, #472, .T. ) ;
#1811 = CARTESIAN_POINT ( 'NONE',  ( -11.06391443747533998, 9.691632641776340762, 38.07293523736174023 ) ) ;
#1812 = CARTESIAN_POINT ( 'NONE',  ( -10.08321815271041544, -9.378998278013590095, 27.91486726096250948 ) ) ;
#1813 = ADVANCED_FACE ( 'NONE', ( #3539 ), #579, .F. ) ;
#1814 = ORIENTED_EDGE ( 'NONE', *, *, #1442, .F. ) ;
#1815 = CARTESIAN_POINT ( 'NONE',  ( 12.00000000000000000, 0.000000000000000000, 35.00000000000000000 ) ) ;
#1816 = VERTEX_POINT ( 'NONE', #2585 ) ;
#1817 = DIRECTION ( 'NONE',  ( 1.000000000000000000, 0.000000000000000000, 0.000000000000000000 ) ) ;
#1818 = DIRECTION ( 'NONE',  ( -0.000000000000000000, -0.000000000000000000, -1.000000000000000000 ) ) ;
#1819 =( LENGTH_UNIT ( ) NAMED_UNIT ( * ) SI_UNIT ( .MILLI., .METRE. ) );
#1820 = VERTEX_POINT ( 'NONE', #3412 ) ;
#1821 = CARTESIAN_POINT ( 'NONE',  ( -9.981067540164714202, 9.981067540164714202, 22.73823205004162418 ) ) ;
#1822 = FACE_OUTER_BOUND ( 'NONE', #2280, .T. ) ;
#1823 = VECTOR ( 'NONE', #491, 999.9999999999998863 ) ;
#1824 = ORIENTED_EDGE ( 'NONE', *, *, #5617, .T. ) ;
#1825 = LINE ( 'NONE', #4166, #1571 ) ;
#1826 = DIRECTION ( 'NONE',  ( 0.000000000000000000, 0.000000000000000000, 1.000000000000000000 ) ) ;
#1827 = PLANE ( 'NONE',  #3255 ) ;
#1828 = SHAPE_REPRESENTATION_RELATIONSHIP ( 'NONE' , 'NONE' ,  #4975, #2480 ) ;
#1829 = VECTOR ( 'NONE', #3742, 1000.000000000000227 ) ;
#1830 = CARTESIAN_POINT ( 'NONE',  ( 9.074396217167732814, -58.26942451214393515, -35.00000000000000000 ) ) ;
#1831 = CARTESIAN_POINT ( 'NONE',  ( 12.74411457810409232, -5.685785403169735019, 35.74643938915853880 ) ) ;
#1832 = CARTESIAN_POINT ( 'NONE',  ( -8.975362584346067152, 9.157688896001753065, 22.85246612729342885 ) ) ;
#1833 = AXIS2_PLACEMENT_3D ( 'NONE', #3217, #4708, #2753 ) ;
#1834 = VERTEX_POINT ( 'NONE', #4412 ) ;
#1835 = VECTOR ( 'NONE', #55, 1000.000000000000000 ) ;
#1836 = CARTESIAN_POINT ( 'NONE',  ( -6.095798759547075285, 10.32656711695237561, 28.09297316833070468 ) ) ;
#1837 = EDGE_LOOP ( 'NONE', ( #3272, #4682, #483, #1175 ) ) ;
#1838 = CARTESIAN_POINT ( 'NONE',  ( 55.48030965893076427, -45.89047003626308197, 35.00000000000000000 ) ) ;
#1839 = EDGE_CURVE ( 'NONE', #2060, #5346, #1515, .T. ) ;
#1840 = ORIENTED_EDGE ( 'NONE', *, *, #2396, .F. ) ;
#1841 = FACE_OUTER_BOUND ( 'NONE', #736, .T. ) ;
#1842 = PRODUCT_DEFINITION_FORMATION_WITH_SPECIFIED_SOURCE ( 'ANY', '', #1404, .NOT_KNOWN. ) ;
#1843 = AXIS2_PLACEMENT_3D ( 'NONE', #881, #5575, #3292 ) ;
#1844 = CARTESIAN_POINT ( 'NONE',  ( 50.91502622129181788, 0.000000000000000000, -35.00000000000000000 ) ) ;
#1845 = CARTESIAN_POINT ( 'NONE',  ( -14.20502198335936050, 3.811938596482205011, 38.16892149784423793 ) ) ;
#1846 = EDGE_CURVE ( 'NONE', #3338, #3265, #682, .T. ) ;
#1847 = EDGE_CURVE ( 'NONE', #720, #3173, #3504, .T. ) ;
#1848 = CARTESIAN_POINT ( 'NONE',  ( 8.983694681928700021, 9.994658916190591214, 22.80938439471025703 ) ) ;
#1849 = ORIENTED_EDGE ( 'NONE', *, *, #3679, .T. ) ;
#1850 = CARTESIAN_POINT ( 'NONE',  ( 57.58482424179643999, 72.37680137756268550, -40.00000000000000000 ) ) ;
#1851 = ORIENTED_EDGE ( 'NONE', *, *, #1592, .T. ) ;
#1852 = DIRECTION ( 'NONE',  ( 1.000000000000000000, 0.000000000000000000, 0.000000000000000000 ) ) ;
#1853 = CARTESIAN_POINT ( 'NONE',  ( -100.0000000000000000, 1.224646799147353217E-14, -39.00000000000002842 ) ) ;
#1854 = VECTOR ( 'NONE', #1246, 1000.000000000000000 ) ;
#1855 = CARTESIAN_POINT ( 'NONE',  ( 0.000000000000000000, 89.46264649666795776, -79.99999999999998579 ) ) ;
#1856 = ORIENTED_EDGE ( 'NONE', *, *, #3921, .T. ) ;
#1857 = EDGE_CURVE ( 'NONE', #705, #3262, #5418, .T. ) ;
#1858 = FACE_BOUND ( 'NONE', #3383, .T. ) ;
#1859 = AXIS2_PLACEMENT_3D ( 'NONE', #5359, #2392, #4282 ) ;
#1860 = CARTESIAN_POINT ( 'NONE',  ( -7.182140071210238271E-14, 8.916303653273167033E-14, -35.00000000000000000 ) ) ;
#1861 = VERTEX_POINT ( 'NONE', #3450 ) ;
#1862 = VECTOR ( 'NONE', #5992, 1000.000000000000000 ) ;
#1863 = VERTEX_POINT ( 'NONE', #5361 ) ;
#1864 = DIRECTION ( 'NONE',  ( -1.000000000000000000, 0.000000000000000000, 0.000000000000000000 ) ) ;
#1865 = DIRECTION ( 'NONE',  ( 1.000000000000000000, 0.000000000000000000, 0.000000000000000000 ) ) ;
#1866 = LINE ( 'NONE', #1405, #5761 ) ;
#1867 = AXIS2_PLACEMENT_3D ( 'NONE', #4906, #1646, #4881 ) ;
#1868 = CARTESIAN_POINT ( 'NONE',  ( 0.000000000000000000, 67.50000000000000000, 20.00000000000000000 ) ) ;
#1869 = EDGE_CURVE ( 'NONE', #5370, #4211, #1158, .T. ) ;
#1870 = CARTESIAN_POINT ( 'NONE',  ( 9.370308891928093686, -8.432825516645548802, 25.44727539999419719 ) ) ;
#1871 = AXIS2_PLACEMENT_3D ( 'NONE', #22, #4840, #2930 ) ;
#1872 = ORIENTED_EDGE ( 'NONE', *, *, #4917, .F. ) ;
#1873 = CARTESIAN_POINT ( 'NONE',  ( -8.539045536263005332, 9.793778397576030414, 27.99842134739334654 ) ) ;
#1874 = ORIENTED_EDGE ( 'NONE', *, *, #4920, .F. ) ;
#1875 = CARTESIAN_POINT ( 'NONE',  ( 8.056095891487838412E-14, -1.254589464284425060E-14, -35.00000000000000000 ) ) ;
#1876 = ORIENTED_EDGE ( 'NONE', *, *, #1260, .T. ) ;
#1877 = DIRECTION ( 'NONE',  ( -1.000000000000000000, 0.000000000000000000, 0.000000000000000000 ) ) ;
#1878 = CARTESIAN_POINT ( 'NONE',  ( -9.858401829237470437, -10.19494410001831497, 33.01259202755186095 ) ) ;
#1879 = CARTESIAN_POINT ( 'NONE',  ( 9.999999999999998224, -9.999999999999998224, 23.00000000000000000 ) ) ;
#1880 = UNCERTAINTY_MEASURE_WITH_UNIT (LENGTH_MEASURE( 1.000000000000000082E-05 ), #923, 'distance_accuracy_value', 'NONE');
#1881 = DIRECTION ( 'NONE',  ( 0.000000000000000000, 0.000000000000000000, -1.000000000000000000 ) ) ;
#1882 = CARTESIAN_POINT ( 'NONE',  ( -6.075059976385840166, -13.36876581604936653, 38.14410695834219922 ) ) ;
#1883 = VERTEX_POINT ( 'NONE', #3044 ) ;
#1884 = CARTESIAN_POINT ( 'NONE',  ( 0.000000000000000000, 0.000000000000000000, -35.00000000000000000 ) ) ;
#1885 = EDGE_CURVE ( 'NONE', #2186, #103, #3012, .T. ) ;
#1886 = DIRECTION ( 'NONE',  ( 0.000000000000000000, 0.000000000000000000, -1.000000000000000000 ) ) ;
#1887 = EDGE_LOOP ( 'NONE', ( #4843, #6138, #1497, #282 ) ) ;
#1888 = LINE ( 'NONE', #2829, #5268 ) ;
#1889 = CARTESIAN_POINT ( 'NONE',  ( 4.666802875123989836, -12.24718835365691127, 33.22501703466258505 ) ) ;
#1890 = ORIENTED_EDGE ( 'NONE', *, *, #2056, .T. ) ;
#1891 = ORIENTED_EDGE ( 'NONE', *, *, #1162, .T. ) ;
#1892 = CARTESIAN_POINT ( 'NONE',  ( 52.58482424179643289, 72.37680137756268550, -79.99999999999998579 ) ) ;
#1893 = EDGE_CURVE ( 'NONE', #1548, #906, #3533, .T. ) ;
#1894 = CARTESIAN_POINT ( 'NONE',  ( 0.000000000000000000, 67.50000000000000000, 20.00000000000000000 ) ) ;
#1895 = PRODUCT_DEFINITION_SHAPE ( 'NONE', 'NONE',  #313 ) ;
#1896 = CARTESIAN_POINT ( 'NONE',  ( -5.114554293134481958E-14, -6.349488965209747807E-14, 35.00000000000000000 ) ) ;
#1897 = CARTESIAN_POINT ( 'NONE',  ( 0.000000000000000000, 0.000000000000000000, 0.000000000000000000 ) ) ;
#1898 = DIRECTION ( 'NONE',  ( -0.000000000000000000, -0.000000000000000000, -1.000000000000000000 ) ) ;
#1899 = CARTESIAN_POINT ( 'NONE',  ( -52.58482424179695158, -72.37680137756228760, -79.99999999999998579 ) ) ;
#1900 = ORIENTED_EDGE ( 'NONE', *, *, #5035, .F. ) ;
#1901 = EDGE_CURVE ( 'NONE', #1611, #5798, #4236, .T. ) ;
#1902 = CARTESIAN_POINT ( 'NONE',  ( 1.716658579843636012, 9.908812303639313868, 25.63028407385522911 ) ) ;
#1903 = CARTESIAN_POINT ( 'NONE',  ( 9.999999999999998224, 9.999999999999998224, 23.00000000000000000 ) ) ;
#1904 = CARTESIAN_POINT ( 'NONE',  ( -14.18603054855838508, -3.792815487222209736, 38.16899780669729125 ) ) ;
#1905 = ORIENTED_EDGE ( 'NONE', *, *, #749, .T. ) ;
#1906 = LINE ( 'NONE', #4785, #1835 ) ;
#1907 = CARTESIAN_POINT ( 'NONE',  ( -8.970286642449650572, -8.321944142006522327, 22.89273687632151066 ) ) ;
#1908 = CARTESIAN_POINT ( 'NONE',  ( 12.00000000000000000, 0.000000000000000000, -35.00000000000000000 ) ) ;
#1909 = CARTESIAN_POINT ( 'NONE',  ( -11.07913919611939058, -71.14248150488579370, 45.00000000000000711 ) ) ;
#1910 = CARTESIAN_POINT ( 'NONE',  ( -68.32682326288350794, 26.05379589900699955, 35.04915833130718994 ) ) ;
#1911 = EDGE_LOOP ( 'NONE', ( #2794, #5809, #5934, #5629, #3854, #578, #3393, #4503, #2809 ) ) ;
#1912 = CYLINDRICAL_SURFACE ( 'NONE', #604, 100.0000000000000000 ) ;
#1913 = EDGE_CURVE ( 'NONE', #3466, #1013, #1447, .T. ) ;
#1914 = DIRECTION ( 'NONE',  ( 0.7787725926866162496, -0.6273063437270228748, 0.000000000000000000 ) ) ;
#1915 = VERTEX_POINT ( 'NONE', #4349 ) ;
#1916 = CARTESIAN_POINT ( 'NONE',  ( 14.48620990986883506, -2.403201876585592256, 38.17751351274289817 ) ) ;
#1917 = CARTESIAN_POINT ( 'NONE',  ( 10.08321815271041899, -9.378998278013591872, 27.91486726096250948 ) ) ;
#1918 = VERTEX_POINT ( 'NONE', #1983 ) ;
#1919 = B_SPLINE_CURVE_WITH_KNOTS ( 'NONE', 3,
 ( #1512, #1034, #31, #5229, #1453, #2886 ),
 .UNSPECIFIED., .F., .F.,
 ( 4, 2, 4 ),
 ( 0.003149728260038243185, 0.01070802693369690868, 0.01826632560735557548 ),
 .UNSPECIFIED. ) ;
#1920 = VERTEX_POINT ( 'NONE', #5795 ) ;
#1921 = CARTESIAN_POINT ( 'NONE',  ( 0.000000000000000000, 89.46264649666795776, -40.00000000000000000 ) ) ;
#1922 = DIRECTION ( 'NONE',  ( 0.000000000000000000, 0.000000000000000000, -1.000000000000000000 ) ) ;
#1923 = CARTESIAN_POINT ( 'NONE',  ( -52.58482424179536707, 72.37680137756343868, -79.99999999999998579 ) ) ;
#1924 = CARTESIAN_POINT ( 'NONE',  ( -19.44593452088801655, 21.33547018489285918, 3.469446951953614189E-15 ) ) ;
#1925 = CARTESIAN_POINT ( 'NONE',  ( 0.000000000000000000, 0.000000000000000000, 40.00000000000000000 ) ) ;
#1926 = CARTESIAN_POINT ( 'NONE',  ( 9.378998278013590095, -10.08321815271041721, 27.91486726096250948 ) ) ;
#1927 = VECTOR ( 'NONE', #424, 1000.000000000000000 ) ;
#1928 = EDGE_CURVE ( 'NONE', #2502, #5015, #5324, .T. ) ;
#1929 = TOROIDAL_SURFACE ( 'NONE', #4825, 72.00000000000004263, 10.00000000000000000 ) ;
#1930 = EDGE_CURVE ( 'NONE', #5851, #103, #2238, .T. ) ;
#1931 = VERTEX_POINT ( 'NONE', #347 ) ;
#1932 = CARTESIAN_POINT ( 'NONE',  ( 7.589415207398531038E-16, 14.74111653287705792, 38.35393095385146012 ) ) ;
#1933 = LINE ( 'NONE', #88, #6040 ) ;
#1935 = AXIS2_PLACEMENT_3D ( 'NONE', #5163, #6067, #1787 ) ;
#1934 = CARTESIAN_POINT ( 'NONE',  ( -11.65565333135050885, -8.931668428568697138, 38.09186409098167303 ) ) ;
#1936 =( REPRESENTATION_RELATIONSHIP ('NONE','NONE', #4716, #4081 ) REPRESENTATION_RELATIONSHIP_WITH_TRANSFORMATION ( #3204 )SHAPE_REPRESENTATION_RELATIONSHIP( ) );
#1937 = VECTOR ( 'NONE', #1031, 1000.000000000000000 ) ;
#1938 = EDGE_LOOP ( 'NONE', ( #1666, #3495, #1750, #5986, #998, #4596 ) ) ;
#1939 = CARTESIAN_POINT ( 'NONE',  ( -74.61196207728360719, -28.86269417393314285, 38.99999999999995737 ) ) ;
#1940 = ADVANCED_FACE ( 'NONE', ( #288 ), #4178, .F. ) ;
#1941 = VECTOR ( 'NONE', #461, 999.9999999999998863 ) ;
#1942 = CARTESIAN_POINT ( 'NONE',  ( -8.967351122863068014, -7.487361748921619764, 22.92808036848186504 ) ) ;
#1943 = AXIS2_PLACEMENT_3D ( 'NONE', #34, #5728, #1010 ) ;
#1944 = CARTESIAN_POINT ( 'NONE',  ( 12.00000000000000000, 50.91502622129181788, -35.00000000000000000 ) ) ;
#1945 = CARTESIAN_POINT ( 'NONE',  ( -15.00000000000000000, 50.91502622129181788, 20.00000000000000000 ) ) ;
#1946 = PRODUCT_DEFINITION_CONTEXT ( 'detailed design', #2778, 'design' ) ;
#1947=STYLED_ITEM('',(#6177),#2173);
#1948 = CARTESIAN_POINT ( 'NONE',  ( 3.000397777471251359, -9.000000000000000000, 23.18288458324515133 ) ) ;
#1949 = CARTESIAN_POINT ( 'NONE',  ( 3.314202382262465996, -14.30535051437892768, 38.17196567842750454 ) ) ;
#1950 = VERTEX_POINT ( 'NONE', #1352 ) ;
#1951 = LINE ( 'NONE', #3809, #4218 ) ;
#1952 = DIRECTION ( 'NONE',  ( 0.000000000000000000, 0.000000000000000000, -1.000000000000000000 ) ) ;
#1953 = CARTESIAN_POINT ( 'NONE',  ( -5.114554293134481958E-14, -6.349488965209747807E-14, 35.00000000000000000 ) ) ;
#1954 = EDGE_LOOP ( 'NONE', ( #5506, #3572, #2381, #2093 ) ) ;
#1955 = DIRECTION ( 'NONE',  ( 1.000000000000000000, 0.000000000000000000, 0.000000000000000000 ) ) ;
#1956 = CARTESIAN_POINT ( 'NONE',  ( 10.04707028972859106, -9.166555234036120936, 25.36260747786040426 ) ) ;
#1957 = ORIENTED_EDGE ( 'NONE', *, *, #2017, .T. ) ;
#1958 = LINE ( 'NONE', #1804, #976 ) ;
#1959 = ORIENTED_EDGE ( 'NONE', *, *, #521, .T. ) ;
#1960 = DIRECTION ( 'NONE',  ( 1.000000000000000000, 0.000000000000000000, 0.000000000000000000 ) ) ;
#1961 = CARTESIAN_POINT ( 'NONE',  ( -46.52501622030217021, -37.47620048660763103, 35.00000000000000000 ) ) ;
#1962 = DIRECTION ( 'NONE',  ( -0.6191766709259440837, 0.7852517113518856506, 0.000000000000000000 ) ) ;
#1963 = DIRECTION ( 'NONE',  ( -0.000000000000000000, -0.000000000000000000, -1.000000000000000000 ) ) ;
#1964 = CARTESIAN_POINT ( 'NONE',  ( 11.57174281757876599, -8.159736356077656794, 35.66679457777021156 ) ) ;
#1965 = CIRCLE ( 'NONE', #1661, 9.999999999999996447 ) ;
#1966 = AXIS2_PLACEMENT_3D ( 'NONE', #3599, #5577, #3202 ) ;
#1967 = ORIENTED_EDGE ( 'NONE', *, *, #2969, .T. ) ;
#1968 = CARTESIAN_POINT ( 'NONE',  ( -1.716690548177159714, 9.908812100099982700, 25.63028262842344773 ) ) ;
#1969 = AXIS2_PLACEMENT_3D ( 'NONE', #4704, #1025, #2904 ) ;
#1970 = CARTESIAN_POINT ( 'NONE',  ( -58.45671475544968843, 33.74999999999987210, -35.00000000000000000 ) ) ;
#1971 = CARTESIAN_POINT ( 'NONE',  ( -11.94400843721153116, -8.542271628753789869, 38.10037361971537706 ) ) ;
#1972 = EDGE_CURVE ( 'NONE', #4835, #5782, #3620, .T. ) ;
#1973 = AXIS2_PLACEMENT_3D ( 'NONE', #3459, #266, #5372 ) ;
#1974 = VERTEX_POINT ( 'NONE', #3256 ) ;
#1975 = DIRECTION ( 'NONE',  ( -0.000000000000000000, 0.000000000000000000, 1.000000000000000000 ) ) ;
#1976 = AXIS2_PLACEMENT_3D ( 'NONE', #5330, #5800, #1159 ) ;
#1977 = ORIENTED_EDGE ( 'NONE', *, *, #1039, .T. ) ;
#1978 = CARTESIAN_POINT ( 'NONE',  ( 9.144590365090015993, -9.969668718019493170, 22.73823205004162773 ) ) ;
#1979 = EDGE_CURVE ( 'NONE', #5045, #3083, #5130, .T. ) ;
#1980 = CARTESIAN_POINT ( 'NONE',  ( -8.999999999988011368, -9.000000000000007105, 23.06137295785747909 ) ) ;
#1981 = LINE ( 'NONE', #3905, #3847 ) ;
#1982 = ORIENTED_EDGE ( 'NONE', *, *, #6125, .F. ) ;
#1983 = CARTESIAN_POINT ( 'NONE',  ( 80.08403291566574467, -27.64547812922912939, -40.00000000000000000 ) ) ;
#1984 = EDGE_CURVE ( 'NONE', #1302, #5383, #2197, .T. ) ;
#1985 = FACE_OUTER_BOUND ( 'NONE', #2365, .T. ) ;
#1986 = DIRECTION ( 'NONE',  ( -0.5000000000000038858, 0.8660254037844362651, 0.000000000000000000 ) ) ;
#1987 = VERTEX_POINT ( 'NONE', #3193 ) ;
#1988 = PRODUCT_DEFINITION_SHAPE ( 'NONE', 'NONE',  #6148 ) ;
#1989 = CARTESIAN_POINT ( 'NONE',  ( 5.685785403169718144, -12.74411457810409765, 35.74643938915854591 ) ) ;
#1990 = EDGE_LOOP ( 'NONE', ( #3199, #3898, #5564, #4576 ) ) ;
#1991 = FACE_OUTER_BOUND ( 'NONE', #3011, .T. ) ;
#1992 = ORIENTED_EDGE ( 'NONE', *, *, #2439, .T. ) ;
#1993 = FACE_OUTER_BOUND ( 'NONE', #5463, .T. ) ;
#1994 = DIRECTION ( 'NONE',  ( 0.7071067811865493491, 8.659560562354955045E-17, -0.7071067811865456854 ) ) ;
#1995 = DIRECTION ( 'NONE',  ( 2.109423746787797427E-15, -1.000000000000000222, 5.824424184503680592E-17 ) ) ;
#1996 = FACE_OUTER_BOUND ( 'NONE', #4497, .T. ) ;
#1997 = CARTESIAN_POINT ( 'NONE',  ( 8.999999999999998224, 8.999999999999998224, -167.0000000000000284 ) ) ;
#1998 = VERTEX_POINT ( 'NONE', #2669 ) ;
#1999 = ORIENTED_EDGE ( 'NONE', *, *, #2983, .T. ) ;
#2000 = CARTESIAN_POINT ( 'NONE',  ( 5.390571672161876826, 11.22195964661421819, 30.65936073406735218 ) ) ;
#2001 = CARTESIAN_POINT ( 'NONE',  ( 10.43169748385510864, 11.73806315776973896, 38.00000000000000711 ) ) ;
#2002 = CARTESIAN_POINT ( 'NONE',  ( -11.04414289254774140, -9.677595944629031166, 38.07286884698770280 ) ) ;
#2003 = ORIENTED_EDGE ( 'NONE', *, *, #5024, .T. ) ;
#2004 = DIRECTION ( 'NONE',  ( 1.000000000000000000, 0.000000000000000000, 0.000000000000000000 ) ) ;
#2005 = CARTESIAN_POINT ( 'NONE',  ( -10.85317354580219273, 1.776706711792239046, 28.17414650202874427 ) ) ;
#2006 = EDGE_LOOP ( 'NONE', ( #6106, #1874, #3024, #1381 ) ) ;
#2007 = CARTESIAN_POINT ( 'NONE',  ( 6.666666666666638541, -9.999999999999998224, 23.00000000000000000 ) ) ;
#2008 = EDGE_CURVE ( 'NONE', #5015, #1165, #3828, .T. ) ;
#2009 = CARTESIAN_POINT ( 'NONE',  ( 8.967351122863068014, 7.487361748921619764, 22.92808036848186504 ) ) ;
#2010 = CARTESIAN_POINT ( 'NONE',  ( -2.411881101062222310, -14.48475173028215401, 38.17746263717076971 ) ) ;
#2011 = ORIENTED_EDGE ( 'NONE', *, *, #4643, .F. ) ;
#2012 = DIRECTION ( 'NONE',  ( -1.000000000000000000, 0.000000000000000000, 0.000000000000000000 ) ) ;
#2013 = FACE_OUTER_BOUND ( 'NONE', #5397, .T. ) ;
#2014 = DIRECTION ( 'NONE',  ( 0.000000000000000000, 0.000000000000000000, 1.000000000000000000 ) ) ;
#2015 = EDGE_CURVE ( 'NONE', #656, #404, #5570, .T. ) ;
#2016 = CARTESIAN_POINT ( 'NONE',  ( 0.000000000000000000, 0.000000000000000000, 38.99999999999995737 ) ) ;
#2017 = EDGE_CURVE ( 'NONE', #747, #2051, #3132, .T. ) ;
#2018 = CARTESIAN_POINT ( 'NONE',  ( 8.926329112024040668, -11.12736491637287806, 35.63514765224429937 ) ) ;
#2019 = ORIENTED_EDGE ( 'NONE', *, *, #6136, .T. ) ;
#2020 = VERTEX_POINT ( 'NONE', #4061 ) ;
#2021 = CARTESIAN_POINT ( 'NONE',  ( 0.000000000000000000, 8.999999999999998224, -167.0000000000000284 ) ) ;
#2022 = CARTESIAN_POINT ( 'NONE',  ( -15.67638808697555142, 0.000000000000000000, 205.0000000000000568 ) ) ;
#2023 = DIRECTION ( 'NONE',  ( 0.000000000000000000, 0.000000000000000000, 1.000000000000000000 ) ) ;
#2024 = DIRECTION ( 'NONE',  ( 0.5000000000000099920, -0.8660254037844329345, 0.000000000000000000 ) ) ;
#2025 = DIRECTION ( 'NONE',  ( 0.000000000000000000, -1.000000000000000000, 0.000000000000000000 ) ) ;
#2026 = ORIENTED_EDGE ( 'NONE', *, *, #1123, .F. ) ;
#2027 = CARTESIAN_POINT ( 'NONE',  ( 2.923529524533198032, 13.51119013911331024, 35.79437308157104525 ) ) ;
#2028 = CARTESIAN_POINT ( 'NONE',  ( 8.309552794738978676, 9.958856949317492990, 22.73823205004162418 ) ) ;
#2029 = FACE_OUTER_BOUND ( 'NONE', #5417, .T. ) ;
#2030 = AXIS2_PLACEMENT_3D ( 'NONE', #4674, #4644, #2804 ) ;
#2031 = ORIENTED_EDGE ( 'NONE', *, *, #1323, .T. ) ;
#2032 = CARTESIAN_POINT ( 'NONE',  ( -1.594625153350711036E-14, -1.594625153350706303E-14, 20.00000000000000000 ) ) ;
#2033 = CARTESIAN_POINT ( 'NONE',  ( -9.871311131128940985, -2.570253631893256951, 25.61911440830482789 ) ) ;
#2034 = AXIS2_PLACEMENT_3D ( 'NONE', #3608, #1254, #1339 ) ;
#2035 = ORIENTED_EDGE ( 'NONE', *, *, #3794, .F. ) ;
#2036 = AXIS2_PLACEMENT_3D ( 'NONE', #5518, #4512, #4580 ) ;
#2037 = CARTESIAN_POINT ( 'NONE',  ( -1.657983872361911803, -9.902916272933980579, 22.73823205004162773 ) ) ;
#2038 = AXIS2_PLACEMENT_3D ( 'NONE', #3997, #2609, #4086 ) ;
#2039 = AXIS2_PLACEMENT_3D ( 'NONE', #2815, #3680, #4241 ) ;
#2040 = CARTESIAN_POINT ( 'NONE',  ( 9.977717576970368540, 7.732441893382015152, 28.03187055541259198 ) ) ;
#2041 = LINE ( 'NONE', #3941, #607 ) ;
#2042 = CIRCLE ( 'NONE', #2447, 15.67638808697555142 ) ;
#2043 = ORIENTED_EDGE ( 'NONE', *, *, #5626, .F. ) ;
#2044 = CARTESIAN_POINT ( 'NONE',  ( -8.056095891487838412E-14, 1.254589464284425060E-14, 35.00000000000000000 ) ) ;
#2045 = EDGE_CURVE ( 'NONE', #354, #4734, #1348, .T. ) ;
#2046 = AXIS2_PLACEMENT_3D ( 'NONE', #4865, #2722, #1756 ) ;
#2047 = EDGE_CURVE ( 'NONE', #2811, #4272, #2698, .T. ) ;
#2048 = DIRECTION ( 'NONE',  ( 0.000000000000000000, 0.000000000000000000, 1.000000000000000000 ) ) ;
#2049 = CARTESIAN_POINT ( 'NONE',  ( 0.8581648076836596584, -9.928243323025412792, 25.63579099555278873 ) ) ;
#2050 = PRESENTATION_LAYER_ASSIGNMENT (  '', '', ( #2849 ) ) ;
#2051 = VERTEX_POINT ( 'NONE', #410 ) ;
#2052 = PLANE ( 'NONE',  #2150 ) ;
#2053 = EDGE_LOOP ( 'NONE', ( #853, #4182, #2832, #4679 ) ) ;
#2054 = DIRECTION ( 'NONE',  ( 1.000000000000000000, 0.000000000000000000, 0.000000000000000000 ) ) ;
#2055 = DIRECTION ( 'NONE',  ( -0.000000000000000000, -0.000000000000000000, 1.000000000000000000 ) ) ;
#2056 = EDGE_CURVE ( 'NONE', #993, #4299, #876, .T. ) ;
#2057 = CARTESIAN_POINT ( 'NONE',  ( -9.306281718482047438, -9.306281718482059873, 25.54332486258996582 ) ) ;
#2058 = CIRCLE ( 'NONE', #4746, 10.00000000000000355 ) ;
#2059 = DIRECTION ( 'NONE',  ( 1.000000000000000000, 0.000000000000000000, 0.000000000000000000 ) ) ;
#2060 = VERTEX_POINT ( 'NONE', #3655 ) ;
#2061 = CARTESIAN_POINT ( 'NONE',  ( 7.732441893382044462, 9.977717576970368540, 28.03187055541259909 ) ) ;
#2062 = CARTESIAN_POINT ( 'NONE',  ( 15.56315586465741774, 2.164213882025733504, 38.00000000000000711 ) ) ;
#2063 = DIRECTION ( 'NONE',  ( -1.000000000000000000, 0.000000000000000000, 0.000000000000000000 ) ) ;
#2064 = EDGE_CURVE ( 'NONE', #5893, #3309, #1786, .T. ) ;
#2065 = VERTEX_POINT ( 'NONE', #2287 ) ;
#2066 = FACE_OUTER_BOUND ( 'NONE', #3648, .T. ) ;
#2067 = CARTESIAN_POINT ( 'NONE',  ( -13.50805179034378867, -5.845970755595367940, 38.28811402100271977 ) ) ;
#2068 = AXIS2_PLACEMENT_3D ( 'NONE', #4722, #478, #2359 ) ;
#2069 = ORIENTED_EDGE ( 'NONE', *, *, #4520, .F. ) ;
#2070 = CARTESIAN_POINT ( 'NONE',  ( 0.8289898103093435999, -9.900940235153619540, 22.73823205004163128 ) ) ;
#2071 = VECTOR ( 'NONE', #5274, 1000.000000000000000 ) ;
#2072 = CARTESIAN_POINT ( 'NONE',  ( 13.11530391916999605, 6.736970939972929173, 38.26632377370044935 ) ) ;
#2073 = VECTOR ( 'NONE', #2378, 1000.000000000000000 ) ;
#2074 = FACE_OUTER_BOUND ( 'NONE', #3507, .T. ) ;
#2075 = EDGE_LOOP ( 'NONE', ( #3887, #5515, #2421, #4317 ) ) ;
#2076 = DIRECTION ( 'NONE',  ( 0.000000000000000000, 0.000000000000000000, 1.000000000000000000 ) ) ;
#2077 = CARTESIAN_POINT ( 'NONE',  ( -1.839547822007357114, -11.79779776130985880, 30.71783115363462002 ) ) ;
#2078 = ORIENTED_EDGE ( 'NONE', *, *, #3761, .T. ) ;
#2079 = CARTESIAN_POINT ( 'NONE',  ( -14.67638808697554964, 0.000000000000000000, 205.0000000000000568 ) ) ;
#2080 = ORIENTED_EDGE ( 'NONE', *, *, #3266, .F. ) ;
#2081 = DIRECTION ( 'NONE',  ( 1.000000000000000000, 0.000000000000000000, 0.000000000000000000 ) ) ;
#2082 = FACE_BOUND ( 'NONE', #2328, .T. ) ;
#2083 = SHAPE_DEFINITION_REPRESENTATION ( #5686, #82 ) ;
#2084 = DIRECTION ( 'NONE',  ( -1.000000000000000000, 0.000000000000000000, 0.000000000000000000 ) ) ;
#2085 = LINE ( 'NONE', #1562, #2481 ) ;
#2086 = EDGE_LOOP ( 'NONE', ( #5666, #2334 ) ) ;
#2087 = EDGE_CURVE ( 'NONE', #3324, #4063, #3707, .T. ) ;
#2088 = ORIENTED_EDGE ( 'NONE', *, *, #5192, .F. ) ;
#2089 = DIRECTION ( 'NONE',  ( -0.000000000000000000, -0.000000000000000000, 1.000000000000000000 ) ) ;
#2090 = PRODUCT_DEFINITION_SHAPE ( 'NONE', 'NONE',  #6151 ) ;
#2091 = DIRECTION ( 'NONE',  ( -0.7071067811865469066, -0.7071067811865482389, 0.000000000000000000 ) ) ;
#2092 = DIRECTION ( 'NONE',  ( 0.000000000000000000, -0.000000000000000000, -1.000000000000000000 ) ) ;
#2093 = ORIENTED_EDGE ( 'NONE', *, *, #1694, .T. ) ;
#2094 = LINE ( 'NONE', #2032, #2125 ) ;
#2095 = ADVANCED_FACE ( 'NONE', ( #3592 ), #789, .F. ) ;
#2096 = CARTESIAN_POINT ( 'NONE',  ( -11.85339260696609287, -0.9193131588476038951, 30.72304697887226510 ) ) ;
#2097 = ORIENTED_EDGE ( 'NONE', *, *, #5913, .F. ) ;
#2098 = CARTESIAN_POINT ( 'NONE',  ( -9.157688896001733525, 8.975362584346067152, 22.85246612729342885 ) ) ;
#2099 = CARTESIAN_POINT ( 'NONE',  ( 0.000000000000000000, 0.000000000000000000, 45.00000000000000711 ) ) ;
#2100 = CARTESIAN_POINT ( 'NONE',  ( -5.000000000000629718, -89.46264649666795776, -79.99999999999998579 ) ) ;
#2101 = VERTEX_POINT ( 'NONE', #2850 ) ;
#2102 = CARTESIAN_POINT ( 'NONE',  ( -4.130675435985315210E-14, -1.067806758184287486E-13, -35.00000000000000000 ) ) ;
#2103 = CARTESIAN_POINT ( 'NONE',  ( -3.879012780925823467, -13.33504572891042272, 35.78373437249953781 ) ) ;
#2104 = ORIENTED_EDGE ( 'NONE', *, *, #181, .T. ) ;
#2105 = LINE ( 'NONE', #1218, #4132 ) ;
#2106 = ORIENTED_EDGE ( 'NONE', *, *, #1558, .T. ) ;
#2107 = DIRECTION ( 'NONE',  ( 1.000000000000000000, 0.000000000000000000, 0.000000000000000000 ) ) ;
#2108 = EDGE_CURVE ( 'NONE', #1042, #4214, #5689, .T. ) ;
#2109 = FACE_OUTER_BOUND ( 'NONE', #3598, .T. ) ;
#2110 = SHAPE_DEFINITION_REPRESENTATION ( #3775, #2176 ) ;
#2111 = DIRECTION ( 'NONE',  ( -0.000000000000000000, -0.000000000000000000, -1.000000000000000000 ) ) ;
#2112 = LINE ( 'NONE', #1616, #5162 ) ;
#2113 = ORIENTED_EDGE ( 'NONE', *, *, #5682, .T. ) ;
#2114 = ORIENTED_EDGE ( 'NONE', *, *, #3542, .F. ) ;
#2115 = CARTESIAN_POINT ( 'NONE',  ( 6.652784304366590185, 8.964415574088988592, 22.96342341013486887 ) ) ;
#2116 = CARTESIAN_POINT ( 'NONE',  ( 11.08488032081241670, -11.08488032081242558, 38.00000000000000000 ) ) ;
#2117 = CARTESIAN_POINT ( 'NONE',  ( 56.07162667343580864, 45.16605674834639217, 45.00000000000000711 ) ) ;
#2118 = EDGE_CURVE ( 'NONE', #1698, #915, #2449, .T. ) ;
#2119 = ADVANCED_FACE ( 'NONE', ( #4686 ), #4342, .T. ) ;
#2120 = ORIENTED_EDGE ( 'NONE', *, *, #4908, .T. ) ;
#2121 = CARTESIAN_POINT ( 'NONE',  ( 0.000000000000000000, 89.46264649666795776, -79.99999999999998579 ) ) ;
#2122 = CARTESIAN_POINT ( 'NONE',  ( -9.638809746143360613, -5.954763795926145242, 25.54536317066256501 ) ) ;
#2123 = VERTEX_POINT ( 'NONE', #2388 ) ;
#2125 = VECTOR ( 'NONE', #5971, 1000.000000000000000 ) ;
#2124 = FACE_OUTER_BOUND ( 'NONE', #5190, .T. ) ;
#2126 = EDGE_CURVE ( 'NONE', #3411, #4200, #3871, .T. ) ;
#2127 = VECTOR ( 'NONE', #2742, 1000.000000000000000 ) ;
#2128 = VECTOR ( 'NONE', #4485, 1000.000000000000000 ) ;
#2129 = CARTESIAN_POINT ( 'NONE',  ( 11.22195964661421641, 5.390571672161841299, 30.65936073406735574 ) ) ;
#2130 = FACE_OUTER_BOUND ( 'NONE', #824, .T. ) ;
#2131 = ORIENTED_EDGE ( 'NONE', *, *, #5100, .F. ) ;
#2132 = VERTEX_POINT ( 'NONE', #3740 ) ;
#2133 = AXIS2_PLACEMENT_3D ( 'NONE', #3258, #4207, #3289 ) ;
#2134 = APPLICATION_CONTEXT ( 'automotive_design' ) ;
#2135 = AXIS2_PLACEMENT_3D ( 'NONE', #346, #5127, #435 ) ;
#2136 = ADVANCED_FACE ( 'NONE', ( #5224 ), #4078, .F. ) ;
#2137 = CARTESIAN_POINT ( 'NONE',  ( 2.570253631893271606, -9.871311131128953420, 25.61911440830483144 ) ) ;
#2138 = AXIS2_PLACEMENT_3D ( 'NONE', #2117, #5501, #775 ) ;
#2139 = CIRCLE ( 'NONE', #2944, 2.499999999999998668 ) ;
#2140 = ORIENTED_EDGE ( 'NONE', *, *, #3040, .F. ) ;
#2141 = FACE_OUTER_BOUND ( 'NONE', #1146, .T. ) ;
#2142 = ORIENTED_EDGE ( 'NONE', *, *, #334, .T. ) ;
#2143 = CARTESIAN_POINT ( 'NONE',  ( 11.33314185117008677, -72.77350886804093477, 35.13717928826310555 ) ) ;
#2144 = VECTOR ( 'NONE', #2555, 999.9999999999998863 ) ;
#2145 = CYLINDRICAL_SURFACE ( 'NONE', #2661, 5.000000000000004441 ) ;
#2146 = PRODUCT_CONTEXT ( 'NONE', #40, 'mechanical' ) ;
#2147 = AXIS2_PLACEMENT_3D ( 'NONE', #4394, #114, #5806 ) ;
#2148 = FACE_OUTER_BOUND ( 'NONE', #2801, .T. ) ;
#2149 = CARTESIAN_POINT ( 'NONE',  ( -80.00000000000000000, 0.000000000000000000, -39.00000000000001421 ) ) ;
#2150 = AXIS2_PLACEMENT_3D ( 'NONE', #5869, #5396, #1136 ) ;
#2151 = VERTEX_POINT ( 'NONE', #623 ) ;
#2152 = CARTESIAN_POINT ( 'NONE',  ( 7.570044180282069490, 12.64059746256323002, 38.23931193745811186 ) ) ;
#2153 = MANIFOLD_SOLID_BREP ( 'Boss-Extrude5', #1354 ) ;
#2154 = CARTESIAN_POINT ( 'NONE',  ( 58.45671475544962448, 33.75000000000001421, 35.00000000000000000 ) ) ;
#2155 = CARTESIAN_POINT ( 'NONE',  ( -9.999999999999998224, 8.999999999999998224, 23.00000000000000000 ) ) ;
#2156 = ORIENTED_EDGE ( 'NONE', *, *, #5112, .T. ) ;
#2157 = DIRECTION ( 'NONE',  ( -0.000000000000000000, 0.000000000000000000, 1.000000000000000000 ) ) ;
#2158 = CARTESIAN_POINT ( 'NONE',  ( -9.370308891928093686, 8.432825516645547026, 25.44727539999419719 ) ) ;
#2159 = EDGE_LOOP ( 'NONE', ( #5816, #5970, #2478, #4338, #4873 ) ) ;
#2160 = CARTESIAN_POINT ( 'NONE',  ( -10.04707028972859106, 9.166555234036119160, 25.36260747786040071 ) ) ;
#2161 = EDGE_CURVE ( 'NONE', #2841, #730, #3939, .T. ) ;
#2162 = DIRECTION ( 'NONE',  ( -0.000000000000000000, 0.000000000000000000, 1.000000000000000000 ) ) ;
#2163 = AXIS2_PLACEMENT_3D ( 'NONE', #2233, #2767, #4133 ) ;
#2164 = CARTESIAN_POINT ( 'NONE',  ( -68.32682326288144736, -26.05379589900766035, 35.04915833130703362 ) ) ;
#2165 = CIRCLE ( 'NONE', #4867, 11.50000000000000178 ) ;
#2166 = DIRECTION ( 'NONE',  ( 0.000000000000000000, -0.000000000000000000, -1.000000000000000000 ) ) ;
#2167 = AXIS2_PLACEMENT_3D ( 'NONE', #5305, #4836, #1369 ) ;
#2168 = EDGE_CURVE ( 'NONE', #2218, #132, #1958, .T. ) ;
#2169 = CARTESIAN_POINT ( 'NONE',  ( -1.131281550719566266E-13, -1.761763928569765259E-14, 35.00000000000000000 ) ) ;
#2170 = EDGE_LOOP ( 'NONE', ( #3479, #2191 ) ) ;
#2171 = EDGE_LOOP ( 'NONE', ( #3457, #2981, #449, #1065, #4049, #2080, #3605, #3551 ) ) ;
#2172 = VECTOR ( 'NONE', #3462, 1000.000000000000000 ) ;
#2173 = MANIFOLD_SOLID_BREP ( 'Fillet1', #5145 ) ;
#2174 = VECTOR ( 'NONE', #709, 1000.000000000000114 ) ;
#2175 = CARTESIAN_POINT ( 'NONE',  ( 1.776762854451772622, -10.85316926984840968, 28.17414535953234278 ) ) ;
#2176 = SHAPE_REPRESENTATION ( 'Die', ( #73 ), #875 ) ;
#2177 = ADVANCED_FACE ( 'NONE', ( #1991 ), #1648, .F. ) ;
#2178 = ORIENTED_EDGE ( 'NONE', *, *, #6011, .T. ) ;
#2179 = CARTESIAN_POINT ( 'NONE',  ( -55.71784976887214924, 21.55374571496067304, -35.00000000000000000 ) ) ;
#2180 = ORIENTED_EDGE ( 'NONE', *, *, #3841, .T. ) ;
#2181 = CARTESIAN_POINT ( 'NONE',  ( 0.000000000000000000, 0.000000000000000000, 35.00000000000000000 ) ) ;
#2182 = DIRECTION ( 'NONE',  ( -0.000000000000000000, -0.000000000000000000, -1.000000000000000000 ) ) ;
#2183 = DIRECTION ( 'NONE',  ( 1.000000000000000000, 0.000000000000000000, 0.000000000000000000 ) ) ;
#2184 = FACE_OUTER_BOUND ( 'NONE', #5323, .T. ) ;
#2185 = CARTESIAN_POINT ( 'NONE',  ( 0.000000000000000000, 0.000000000000000000, 38.99999999999995737 ) ) ;
#2186 = VERTEX_POINT ( 'NONE', #4834 ) ;
#2187 = LINE ( 'NONE', #4076, #1862 ) ;
#2188 = CARTESIAN_POINT ( 'NONE',  ( -9.074396217167167933, -58.26942451214404173, -35.00000000000000000 ) ) ;
#2189 = CARTESIAN_POINT ( 'NONE',  ( 9.999999999999998224, -0.8333333333333816650, 23.00000000000000000 ) ) ;
#2190 = CARTESIAN_POINT ( 'NONE',  ( 0.000000000000000000, 0.000000000000000000, -35.00000000000000000 ) ) ;
#2191 = ORIENTED_EDGE ( 'NONE', *, *, #2710, .F. ) ;
#2192 = CARTESIAN_POINT ( 'NONE',  ( 9.708537589994000072, -5.113933401365548193, 25.56820946177495557 ) ) ;
#2193 = CARTESIAN_POINT ( 'NONE',  ( -8.963431154120575783, 4.154433491267528922, 23.04275521548131067 ) ) ;
#2194 = ORIENTED_EDGE ( 'NONE', *, *, #5522, .F. ) ;
#2195 = FACE_OUTER_BOUND ( 'NONE', #5178, .T. ) ;
#2196 = B_SPLINE_SURFACE_WITH_KNOTS ( 'NONE', 3, 1, ( 
 ( #1591, #3489, #5402 ),
 ( #5022, #5144, #770 ),
 ( #888, #6049, #4670 ),
 ( #420, #4549, #2235 ),
 ( #333, #1249, #5519 ),
 ( #2769, #2652, #4189 ),
 ( #857, #3146, #4639 ),
 ( #2209, #1225, #5553 ),
 ( #5111, #4163, #5056 ),
 ( #4100, #1796, #4581 ),
 ( #2736, #304, #1332 ),
 ( #5580, #805, #6016 ),
 ( #4073, #5991, #359 ),
 ( #3237, #834, #2709 ),
 ( #2682, #388, #2269 ),
 ( #6075, #3693, #5605 ),
 ( #2298, #1770, #6104 ),
 ( #1732, #1306, #1821 ) ),
 .UNSPECIFIED., .F., .F., .F.,
 ( 4, 2, 2, 2, 2, 2, 2, 2, 4 ),
 ( 2, 1, 2 ),
 ( 0.000000000000000000, 0.1250000000000000833, 0.2500000000000001665, 0.3750000000000001110, 0.5000000000000001110, 0.6250000000000001110, 0.7500000000000000000, 0.8750000000000000000, 1.000000000000000000 ),
 ( 0.000000000000000000, 1.000000000000000000, 1.017451196663891722 ),
 .UNSPECIFIED. ) ;
#2197 = LINE ( 'NONE', #4625, #4943 ) ;
#2198 = FACE_OUTER_BOUND ( 'NONE', #4368, .T. ) ;
#2199 = EDGE_LOOP ( 'NONE', ( #3949, #5614, #2647, #1055 ) ) ;
#2200 = EDGE_CURVE ( 'NONE', #836, #2604, #4440, .T. ) ;
#2201 = CARTESIAN_POINT ( 'NONE',  ( -7.610208295502499887, -9.462636878983104793, 25.48187184588751819 ) ) ;
#2202 = VERTEX_POINT ( 'NONE', #4874 ) ;
#2203 = CARTESIAN_POINT ( 'NONE',  ( -80.99999999999998579, 0.000000000000000000, -40.00000000000000000 ) ) ;
#2204 = VERTEX_POINT ( 'NONE', #3700 ) ;
#2205 = DIRECTION ( 'NONE',  ( 1.000000000000000000, 0.000000000000000000, 0.000000000000000000 ) ) ;
#2206 = CARTESIAN_POINT ( 'NONE',  ( -8.999999999999998224, -9.999999999999998224, 23.00000000000000000 ) ) ;
#2207 = DIRECTION ( 'NONE',  ( -0.8660254037844339337, -0.5000000000000079936, 0.000000000000000000 ) ) ;
#2208 = EDGE_CURVE ( 'NONE', #2569, #1495, #3344, .T. ) ;
#2209 = CARTESIAN_POINT ( 'NONE',  ( -15.56315586465741951, -2.164213882025732172, 38.00000000000000711 ) ) ;
#2210 = DIRECTION ( 'NONE',  ( 1.000000000000000000, 0.000000000000000000, 0.000000000000000000 ) ) ;
#2211 = ORIENTED_EDGE ( 'NONE', *, *, #1200, .T. ) ;
#2212 = CARTESIAN_POINT ( 'NONE',  ( 25.10043906316099083, 27.60043906316109386, 35.00000000000000000 ) ) ;
#2213 = DIRECTION ( 'NONE',  ( 0.000000000000000000, 0.000000000000000000, 1.000000000000000000 ) ) ;
#2214 = LINE ( 'NONE', #4168, #2958 ) ;
#2215 =( NAMED_UNIT ( * ) PLANE_ANGLE_UNIT ( ) SI_UNIT ( $, .RADIAN. ) );
#2216 = CARTESIAN_POINT ( 'NONE',  ( 11.58281169573755953, -3.645573174172184405, 30.69674159737795449 ) ) ;
#2217 = CARTESIAN_POINT ( 'NONE',  ( -9.708537589994000072, 5.113933401365539311, 25.56820946177495557 ) ) ;
#2218 = VERTEX_POINT ( 'NONE', #5016 ) ;
#2219 = CARTESIAN_POINT ( 'NONE',  ( -4.807938790076510926, 13.07368784376655491, 35.76776929191790089 ) ) ;
#2220 = DIRECTION ( 'NONE',  ( -0.000000000000000000, -0.000000000000000000, 1.000000000000000000 ) ) ;
#2221 = CARTESIAN_POINT ( 'NONE',  ( -8.056095891487838412E-14, 1.254589464284425060E-14, 35.00000000000000000 ) ) ;
#2222 = CARTESIAN_POINT ( 'NONE',  ( 11.07913919612032316, -71.14248150488565159, 45.00000000000000711 ) ) ;
#2223 = VERTEX_POINT ( 'NONE', #679 ) ;
#2224 = AXIS2_PLACEMENT_3D ( 'NONE', #4077, #5993, #6022 ) ;
#2225 = CARTESIAN_POINT ( 'NONE',  ( -10.19494410001831142, -9.858401829237470437, 33.01259202755186095 ) ) ;
#2226 = ORIENTED_EDGE ( 'NONE', *, *, #605, .T. ) ;
#2227 = CARTESIAN_POINT ( 'NONE',  ( 80.00000000000000000, 9.797174393178826052E-15, -39.00000000000001421 ) ) ;
#2228 = ORIENTED_EDGE ( 'NONE', *, *, #2759, .F. ) ;
#2229 = DIRECTION ( 'NONE',  ( 0.000000000000000000, 0.000000000000000000, 1.000000000000000000 ) ) ;
#2230 = EDGE_CURVE ( 'NONE', #3051, #3466, #4948, .T. ) ;
#2231 = VECTOR ( 'NONE', #5962, 1000.000000000000000 ) ;
#2232 = EDGE_CURVE ( 'NONE', #5114, #4690, #261, .T. ) ;
#2233 = CARTESIAN_POINT ( 'NONE',  ( 0.000000000000000000, 0.000000000000000000, 205.0000000000000568 ) ) ;
#2234 = DIRECTION ( 'NONE',  ( -0.000000000000000000, 0.000000000000000000, 1.000000000000000000 ) ) ;
#2235 = CARTESIAN_POINT ( 'NONE',  ( -9.939337621248920840, -6.642184745761411158, 22.73823205004162418 ) ) ;
#2236 = AXIS2_PLACEMENT_3D ( 'NONE', #3837, #4853, #4340 ) ;
#2237 = DIRECTION ( 'NONE',  ( 1.000000000000000000, 0.000000000000000000, 0.000000000000000000 ) ) ;
#2238 = CIRCLE ( 'NONE', #2046, 5.000000000000004441 ) ;
#2239 = VERTEX_POINT ( 'NONE', #3978 ) ;
#2240 = PLANE ( 'NONE',  #5258 ) ;
#2241 = ADVANCED_FACE ( 'NONE', ( #5049 ), #1639, .F. ) ;
#2242 = CARTESIAN_POINT ( 'NONE',  ( -80.08403291566614257, -27.64547812922793923, -79.99999999999998579 ) ) ;
#2243 = DIRECTION ( 'NONE',  ( -0.6273063437270329779, 0.7787725926866080339, 0.000000000000000000 ) ) ;
#2244 = ORIENTED_EDGE ( 'NONE', *, *, #5192, .T. ) ;
#2245 =( LENGTH_UNIT ( ) NAMED_UNIT ( * ) SI_UNIT ( .MILLI., .METRE. ) );
#2246 = VECTOR ( 'NONE', #3017, 1000.000000000000000 ) ;
#2247 = CARTESIAN_POINT ( 'NONE',  ( 9.871311131128940985, -2.570253631893350210, 25.61911440830482789 ) ) ;
#2248 = CARTESIAN_POINT ( 'NONE',  ( -12.60026679007841466, 2.830884587392776819, 33.25110354061416018 ) ) ;
#2249 = ORIENTED_EDGE ( 'NONE', *, *, #4446, .T. ) ;
#2250 = EDGE_CURVE ( 'NONE', #1863, #4386, #1673, .T. ) ;
#2251 = CARTESIAN_POINT ( 'NONE',  ( -2.491918585145397991, 8.964680801521355491, 23.07363600708416129 ) ) ;
#2252 = DIRECTION ( 'NONE',  ( 1.000000000000000000, 0.000000000000000000, 0.000000000000000000 ) ) ;
#2253 = DIRECTION ( 'NONE',  ( -0.000000000000000000, -0.000000000000000000, 1.000000000000000000 ) ) ;
#2254 =( REPRESENTATION_RELATIONSHIP ('NONE','NONE', #4716, #4081 ) REPRESENTATION_RELATIONSHIP_WITH_TRANSFORMATION ( #3143 )SHAPE_REPRESENTATION_RELATIONSHIP( ) );
#2255 = CARTESIAN_POINT ( 'NONE',  ( 0.000000000000000000, -8.999999999999998224, -167.0000000000000284 ) ) ;
#2256 = CIRCLE ( 'NONE', #5551, 72.00000000000004263 ) ;
#2257 = CARTESIAN_POINT ( 'NONE',  ( -1.630640067418198669E-13, 67.50000000000002842, 35.00000000000000000 ) ) ;
#2258 = CIRCLE ( 'NONE', #5756, 12.49999999999999822 ) ;
#2259 = VECTOR ( 'NONE', #5084, 1000.000000000000000 ) ;
#2260 = CARTESIAN_POINT ( 'NONE',  ( -5.533593864557681208, -11.98089146579572883, 33.20390238845318009 ) ) ;
#2261 = VERTEX_POINT ( 'NONE', #2562 ) ;
#2262 = LINE ( 'NONE', #1326, #3361 ) ;
#2263 = VECTOR ( 'NONE', #5671, 1000.000000000000000 ) ;
#2264 = ORIENTED_EDGE ( 'NONE', *, *, #2594, .F. ) ;
#2265 = CARTESIAN_POINT ( 'NONE',  ( -47.58482424179695158, -72.37680137756228760, 40.00000000000000000 ) ) ;
#2266 = CARTESIAN_POINT ( 'NONE',  ( 54.99999999999999289, 6.349087922075113966E-13, 35.00000000000000000 ) ) ;
#2267 = CONTEXT_DEPENDENT_SHAPE_REPRESENTATION ( #368, #5389 ) ;
#2268 = PLANE ( 'NONE',  #2638 ) ;
#2269 = CARTESIAN_POINT ( 'NONE',  ( -9.939337621248920840, 6.642184745761469777, 22.73823205004162418 ) ) ;
#2270 = VECTOR ( 'NONE', #4345, 1000.000000000000000 ) ;
#2271 = CARTESIAN_POINT ( 'NONE',  ( 68.69027832784067300, -26.57196568621440491, 35.00000000000000000 ) ) ;
#2272 = VERTEX_POINT ( 'NONE', #2646 ) ;
#2273 = DIRECTION ( 'NONE',  ( 0.1538769332794418798, -0.9880900209011901358, 0.000000000000000000 ) ) ;
#2274 = CARTESIAN_POINT ( 'NONE',  ( 46.52501622030217021, 37.47620048660763103, 35.00000000000000000 ) ) ;
#2275 = CARTESIAN_POINT ( 'NONE',  ( 9.692295192625326905, 11.06325188662640180, 38.07291408809467015 ) ) ;
#2276 = SHAPE_REPRESENTATION_RELATIONSHIP ( 'NONE' , 'NONE' ,  #4081, #3579 ) ;
#2277 = CARTESIAN_POINT ( 'NONE',  ( 10.89081796499577237, -0.8880320553140826911, 28.17941898721253580 ) ) ;
#2278 = ADVANCED_FACE ( 'NONE', ( #4958 ), #2747, .F. ) ;
#2279 = CARTESIAN_POINT ( 'NONE',  ( -8.965240787521256749, 1.660914622755444991, 23.08598164463087343 ) ) ;
#2280 = EDGE_LOOP ( 'NONE', ( #5885, #799, #1647, #2561 ) ) ;
#2281 = CARTESIAN_POINT ( 'NONE',  ( -5.845970755595359947, 13.50805179034379044, 38.28811402100272687 ) ) ;
#2282 = CARTESIAN_POINT ( 'NONE',  ( 0.000000000000000000, 0.000000000000000000, 35.00000000000000000 ) ) ;
#2283 = ORIENTED_EDGE ( 'NONE', *, *, #1006, .F. ) ;
#2284 = EDGE_CURVE ( 'NONE', #15, #4405, #3057, .T. ) ;
#2285 = CARTESIAN_POINT ( 'NONE',  ( -85.08403291566612836, -27.64547812922793923, -79.99999999999998579 ) ) ;
#2286 = ADVANCED_FACE ( 'NONE', ( #2141 ), #3109, .F. ) ;
#2287 = CARTESIAN_POINT ( 'NONE',  ( -12.49999999999999822, -67.50000000000000000, -35.00000000000000000 ) ) ;
#2288 = CARTESIAN_POINT ( 'NONE',  ( -7.182140071210238271E-14, 8.916303653273167033E-14, -35.00000000000000000 ) ) ;
#2289 = CARTESIAN_POINT ( 'NONE',  ( -9.632247231687292910, -10.63625351335941716, 35.59852902770369809 ) ) ;
#2290 = VERTEX_POINT ( 'NONE', #5490 ) ;
#2291 = CARTESIAN_POINT ( 'NONE',  ( 30.10043906316099083, 27.60043906316109386, 35.00000000000000000 ) ) ;
#2292 = ORIENTED_EDGE ( 'NONE', *, *, #1928, .F. ) ;
#2293 = CARTESIAN_POINT ( 'NONE',  ( -6.247143215332724651E-13, -89.46264649666795776, 40.00000000000000000 ) ) ;
#2294 = DIRECTION ( 'NONE',  ( 0.000000000000000000, 0.000000000000000000, 1.000000000000000000 ) ) ;
#2295 = ITEM_DEFINED_TRANSFORMATION ( 'NONE', 'NONE', #972,  #73 ) ;
#2296 = DIRECTION ( 'NONE',  ( 0.000000000000000000, 0.000000000000000000, 1.000000000000000000 ) ) ;
#2297 = VERTEX_POINT ( 'NONE', #4928 ) ;
#2298 = CARTESIAN_POINT ( 'NONE',  ( -11.73806315776973364, 10.43169748385510864, 38.00000000000000000 ) ) ;
#2299 = DIRECTION ( 'NONE',  ( -0.000000000000000000, -0.000000000000000000, 1.000000000000000000 ) ) ;
#2300 = PRODUCT_DEFINITION ( 'UNKNOWN', '', #3728, #5691 ) ;
#2301 = ORIENTED_EDGE ( 'NONE', *, *, #320, .F. ) ;
#2302 = CARTESIAN_POINT ( 'NONE',  ( 1.131281550719567528E-13, 1.761763928569687004E-14, 35.00000000000000000 ) ) ;
#2303 = CARTESIAN_POINT ( 'NONE',  ( 58.45671475544992290, -33.74999999999945999, -35.00000000000000000 ) ) ;
#2304 = CARTESIAN_POINT ( 'NONE',  ( 8.952355667640917503, 11.66870637430316648, 38.09164563373214918 ) ) ;
#2305 = SHAPE_REPRESENTATION_RELATIONSHIP ( 'NONE' , 'NONE' ,  #82, #6110 ) ;
#2306 = CARTESIAN_POINT ( 'NONE',  ( 13.77854189090673742, -1.299091064715344294E-14, 35.81030296219172726 ) ) ;
#2307 =( LENGTH_UNIT ( ) NAMED_UNIT ( * ) SI_UNIT ( .MILLI., .METRE. ) );
#2308 = ORIENTED_EDGE ( 'NONE', *, *, #3198, .T. ) ;
#2309 = CARTESIAN_POINT ( 'NONE',  ( -5.247549479766024483, 10.46302782743270754, 28.11481907968152427 ) ) ;
#2310 = CARTESIAN_POINT ( 'NONE',  ( 56.10121673609980064, -46.04269404270027621, 35.00000000000000000 ) ) ;
#2311 = EDGE_CURVE ( 'NONE', #1644, #6134, #5736, .T. ) ;
#2312 = ADVANCED_FACE ( 'NONE', ( #233 ), #3139, .F. ) ;
#2313 = ORIENTED_EDGE ( 'NONE', *, *, #5292, .F. ) ;
#2314 = B_SPLINE_CURVE_WITH_KNOTS ( 'NONE', 3,
 ( #3882, #4869, #619, #1350, #820, #2315 ),
 .UNSPECIFIED., .F., .F.,
 ( 4, 2, 4 ),
 ( 0.002357188415687185273, 0.01135824717474477781, 0.02035930593380236991 ),
 .UNSPECIFIED. ) ;
#2315 = CARTESIAN_POINT ( 'NONE',  ( 8.999999999988068211, 9.000000000000005329, 23.06137295785747554 ) ) ;
#2316 = DIRECTION ( 'NONE',  ( 0.000000000000000000, -1.000000000000000000, 0.000000000000000000 ) ) ;
#2317 = CARTESIAN_POINT ( 'NONE',  ( -14.67638808697555319, 1.484446970801598990E-11, 38.18288438803429585 ) ) ;
#2318 = EDGE_CURVE ( 'NONE', #5138, #5202, #2105, .T. ) ;
#2319 = DIRECTION ( 'NONE',  ( 0.000000000000000000, 0.000000000000000000, -1.000000000000000000 ) ) ;
#2320 = ORIENTED_EDGE ( 'NONE', *, *, #1162, .F. ) ;
#2321 = DIRECTION ( 'NONE',  ( -0.1538769332794418798, 0.9880900209011901358, 0.000000000000000000 ) ) ;
#2322 = VERTEX_POINT ( 'NONE', #5461 ) ;
#2323 = DIRECTION ( 'NONE',  ( 0.000000000000000000, -1.000000000000000000, 0.000000000000000000 ) ) ;
#2324 = EDGE_CURVE ( 'NONE', #764, #2290, #4989, .T. ) ;
#2325 = LINE ( 'NONE', #2860, #6047 ) ;
#2326 = CIRCLE ( 'NONE', #5820, 72.00000000000004263 ) ;
#2327 = SURFACE_STYLE_USAGE ( .BOTH. , #445 ) ;
#2328 = EDGE_LOOP ( 'NONE', ( #1206, #650 ) ) ;
#2329 = FACE_BOUND ( 'NONE', #4907, .T. ) ;
#2330 = DIRECTION ( 'NONE',  ( 1.000000000000000000, 0.000000000000000000, 0.000000000000000000 ) ) ;
#2331 = VECTOR ( 'NONE', #4361, 1000.000000000000000 ) ;
#2332 = VECTOR ( 'NONE', #941, 1000.000000000000000 ) ;
#2333 = ORIENTED_EDGE ( 'NONE', *, *, #635, .T. ) ;
#2334 = ORIENTED_EDGE ( 'NONE', *, *, #3710, .T. ) ;
#2335 = CARTESIAN_POINT ( 'NONE',  ( 55.00000000000024158, -21.27605460799916770, 35.00000000000000000 ) ) ;
#2336 = LINE ( 'NONE', #2470, #2331 ) ;
#2337 = CARTESIAN_POINT ( 'NONE',  ( -55.00000000000010658, 21.27605460799956205, 35.00000000000000000 ) ) ;
#2338 = VECTOR ( 'NONE', #819, 1000.000000000000114 ) ;
#2339 = CARTESIAN_POINT ( 'NONE',  ( 9.306281718482082965, 9.306281718482070531, 25.54332486258998358 ) ) ;
#2340 = AXIS2_PLACEMENT_3D ( 'NONE', #5539, #2755, #3617 ) ;
#2341 = CARTESIAN_POINT ( 'NONE',  ( 5.141101056459331353, 67.50000000000000000, -28.99999999999999645 ) ) ;
#2342 = AXIS2_PLACEMENT_3D ( 'NONE', #4635, #3141, #4131 ) ;
#2343 = AXIS2_PLACEMENT_3D ( 'NONE', #5785, #4886, #2512 ) ;
#2344 = ORIENTED_EDGE ( 'NONE', *, *, #5176, .T. ) ;
#2345 = CARTESIAN_POINT ( 'NONE',  ( -8.159736356077649688, 11.57174281757876777, 35.66679457777021867 ) ) ;
#2346 = VERTEX_POINT ( 'NONE', #2179 ) ;
#2347 = DIRECTION ( 'NONE',  ( 0.000000000000000000, 0.000000000000000000, 1.000000000000000000 ) ) ;
#2348 = AXIS2_PLACEMENT_3D ( 'NONE', #2525, #1607, #1132 ) ;
#2349 = EDGE_LOOP ( 'NONE', ( #2078, #3913, #3960, #648 ) ) ;
#2350 = FACE_OUTER_BOUND ( 'NONE', #1585, .T. ) ;
#2351 =( GEOMETRIC_REPRESENTATION_CONTEXT ( 3 ) GLOBAL_UNCERTAINTY_ASSIGNED_CONTEXT ( ( #847 ) ) GLOBAL_UNIT_ASSIGNED_CONTEXT ( ( #5340, #1467, #2872 ) ) REPRESENTATION_CONTEXT ( 'NONE', 'WORKASPACE' ) );
#2352 = EDGE_CURVE ( 'NONE', #5798, #4467, #5363, .T. ) ;
#2353 = CARTESIAN_POINT ( 'NONE',  ( -12.11088206474084572, -8.328520801854336852, 38.20782360758019536 ) ) ;
#2354 = DIRECTION ( 'NONE',  ( 0.000000000000000000, 0.000000000000000000, 1.000000000000000000 ) ) ;
#2355 = ADVANCED_FACE ( 'NONE', ( #172 ), #2052, .F. ) ;
#2356 = LINE ( 'NONE', #3876, #2270 ) ;
#2357 = VECTOR ( 'NONE', #2375, 1000.000000000000000 ) ;
#2358 = ORIENTED_EDGE ( 'NONE', *, *, #4339, .F. ) ;
#2359 = DIRECTION ( 'NONE',  ( 1.000000000000000000, 0.000000000000000000, 0.000000000000000000 ) ) ;
#2360 = ORIENTED_EDGE ( 'NONE', *, *, #1737, .F. ) ;
#2361 = DIRECTION ( 'NONE',  ( -0.000000000000000000, -0.000000000000000000, 1.000000000000000000 ) ) ;
#2362 = CARTESIAN_POINT ( 'NONE',  ( -12.31015466235495026, -79.04720167209526949, 35.00000000000000000 ) ) ;
#2363 = CIRCLE ( 'NONE', #5859, 15.67638808697555142 ) ;
#2364 = PLANE ( 'NONE',  #3812 ) ;
#2365 = EDGE_LOOP ( 'NONE', ( #1019, #2019 ) ) ;
#2366 = CARTESIAN_POINT ( 'NONE',  ( 13.16326790094642263, -6.508032323544555631, 38.13839276770974607 ) ) ;
#2367 = EDGE_CURVE ( 'NONE', #5096, #962, #5242, .T. ) ;
#2368 = VECTOR ( 'NONE', #5106, 1000.000000000000114 ) ;
#2369 = CARTESIAN_POINT ( 'NONE',  ( 8.007183658747738519, -11.03292118881348394, 33.12420745160152791 ) ) ;
#2370 = VERTEX_POINT ( 'NONE', #2227 ) ;
#2371 = CIRCLE ( 'NONE', #4558, 5.000000000000004441 ) ;
#2372 = ORIENTED_EDGE ( 'NONE', *, *, #2232, .F. ) ;
#2373 = LINE ( 'NONE', #1498, #1102 ) ;
#2374 = CARTESIAN_POINT ( 'NONE',  ( -8.999999999999998224, -8.999999999999998224, 23.00000000000000000 ) ) ;
#2375 = DIRECTION ( 'NONE',  ( -0.000000000000000000, -0.000000000000000000, -1.000000000000000000 ) ) ;
#2376 = DIRECTION ( 'NONE',  ( 5.551115123125782702E-17, -1.387778780781445676E-17, 1.000000000000000000 ) ) ;
#2377 = CIRCLE ( 'NONE', #806, 10.00000000000000178 ) ;
#2378 = DIRECTION ( 'NONE',  ( -0.000000000000000000, -0.000000000000000000, -1.000000000000000000 ) ) ;
#2379 = CARTESIAN_POINT ( 'NONE',  ( 11.12726264164139245, -8.926511697459380557, 35.63515070857870626 ) ) ;
#2380 = AXIS2_PLACEMENT_3D ( 'NONE', #180, #2966, #3461 ) ;
#2381 = ORIENTED_EDGE ( 'NONE', *, *, #4137, .T. ) ;
#2382 = CARTESIAN_POINT ( 'NONE',  ( 3.759380242563083563, 12.45811160333930800, 33.24069127598783524 ) ) ;
#2383 = CARTESIAN_POINT ( 'NONE',  ( 4.260267006495017661, 15.12434353048566749, 38.00000000000000711 ) ) ;
#2384 = DIRECTION ( 'NONE',  ( 0.000000000000000000, 0.000000000000000000, 1.000000000000000000 ) ) ;
#2385 =( REPRESENTATION_RELATIONSHIP ('NONE','NONE', #4716, #4081 ) REPRESENTATION_RELATIONSHIP_WITH_TRANSFORMATION ( #1729 )SHAPE_REPRESENTATION_RELATIONSHIP( ) );
#2386 = EDGE_LOOP ( 'NONE', ( #2104, #664, #3640, #119 ) ) ;
#2387 = DIRECTION ( 'NONE',  ( 0.000000000000000000, -0.000000000000000000, -1.000000000000000000 ) ) ;
#2388 = CARTESIAN_POINT ( 'NONE',  ( 4.999999999999380940, -89.46264649666795776, 40.00000000000000000 ) ) ;
#2389 = B_SPLINE_CURVE_WITH_KNOTS ( 'NONE', 3,
 ( #1980, #2854, #5792, #1948, #3, #4760 ),
 .UNSPECIFIED., .F., .F.,
 ( 4, 2, 4 ),
 ( 0.002357188415687252060, 0.01135824717474482638, 0.02035930593380240114 ),
 .UNSPECIFIED. ) ;
#2390 = CARTESIAN_POINT ( 'NONE',  ( -11.66987820548587074, 8.950926204225673644, 38.09167945787530840 ) ) ;
#2391 = CARTESIAN_POINT ( 'NONE',  ( 10.63625351335941893, 9.632247231687287581, 35.59852902770369099 ) ) ;
#2392 = DIRECTION ( 'NONE',  ( 0.000000000000000000, 0.000000000000000000, 1.000000000000000000 ) ) ;
#2393 = VERTEX_POINT ( 'NONE', #4129 ) ;
#2394 = CARTESIAN_POINT ( 'NONE',  ( 6.314393452555577824E-13, -67.50000000000002842, 35.00000000000000000 ) ) ;
#2395 = FACE_OUTER_BOUND ( 'NONE', #4321, .T. ) ;
#2396 = EDGE_CURVE ( 'NONE', #962, #5096, #3147, .T. ) ;
#2397 = EDGE_CURVE ( 'NONE', #5277, #4214, #3713, .T. ) ;
#2398 = FACE_OUTER_BOUND ( 'NONE', #3403, .T. ) ;
#2399 = ORIENTED_EDGE ( 'NONE', *, *, #2427, .T. ) ;
#2400 = CARTESIAN_POINT ( 'NONE',  ( 58.45671475544992290, -33.74999999999945999, 35.00000000000000000 ) ) ;
#2401 = CARTESIAN_POINT ( 'NONE',  ( 3.531709963121631102, -10.70751606408959589, 28.15279306126448589 ) ) ;
#2402 = ORIENTED_EDGE ( 'NONE', *, *, #4759, .T. ) ;
#2403 = ORIENTED_EDGE ( 'NONE', *, *, #3155, .T. ) ;
#2404 = FACE_OUTER_BOUND ( 'NONE', #5902, .T. ) ;
#2405 = CARTESIAN_POINT ( 'NONE',  ( 15.00000000000000000, 50.91502622129181788, 20.00000000000000000 ) ) ;
#2406 = CARTESIAN_POINT ( 'NONE',  ( -2.941541598353333735E-14, 7.604078429494112756E-14, 35.00000000000000000 ) ) ;
#2407 = DIRECTION ( 'NONE',  ( -0.8966476046699525249, 0.4427449299987936127, 5.551115123125782702E-17 ) ) ;
#2408 = ADVANCED_FACE ( 'NONE', ( #3687 ), #1357, .F. ) ;
#2409 = DIRECTION ( 'NONE',  ( 1.000000000000000000, 0.000000000000000000, 0.000000000000000000 ) ) ;
#2410 = CARTESIAN_POINT ( 'NONE',  ( 9.269614772507654976, -9.245260337044141963, 25.40693856330804223 ) ) ;
#2411 = VERTEX_POINT ( 'NONE', #2291 ) ;
#2412 = CARTESIAN_POINT ( 'NONE',  ( 5.954811582427137040, 9.638809502600501844, 25.54535933516314117 ) ) ;
#2413 = CARTESIAN_POINT ( 'NONE',  ( 4.147343260682193389, 9.916251082295017838, 22.73823205004162418 ) ) ;
#2414 = FACE_OUTER_BOUND ( 'NONE', #5765, .T. ) ;
#2415 = EDGE_LOOP ( 'NONE', ( #4852, #3503, #3974, #4421 ) ) ;
#2416 = PLANE ( 'NONE',  #2723 ) ;
#2417 = CARTESIAN_POINT ( 'NONE',  ( -9.378998278013590095, -10.08321815271042432, 27.91486726096250948 ) ) ;
#2418 = CARTESIAN_POINT ( 'NONE',  ( -3.333333333333376558, -9.999999999999998224, 23.00000000000000000 ) ) ;
#2419 = DIRECTION ( 'NONE',  ( -0.1538769332794359679, -0.9880900209011910240, 0.000000000000000000 ) ) ;
#2420 = CARTESIAN_POINT ( 'NONE',  ( 0.000000000000000000, 0.000000000000000000, 35.00000000000000000 ) ) ;
#2421 = ORIENTED_EDGE ( 'NONE', *, *, #2558, .T. ) ;
#2422 = CARTESIAN_POINT ( 'NONE',  ( 10.37777353962571425, 10.37777353962603044, 38.05103295300744293 ) ) ;
#2423 = DIRECTION ( 'NONE',  ( -1.000000000000000000, 0.000000000000000000, 0.000000000000000000 ) ) ;
#2424 = ORIENTED_EDGE ( 'NONE', *, *, #5419, .T. ) ;
#2425 = CARTESIAN_POINT ( 'NONE',  ( 14.20502198335932142, -3.811938596482332020, 38.16892149784424504 ) ) ;
#2426 = CARTESIAN_POINT ( 'NONE',  ( 3.423816715609377948, -9.833810162157929469, 25.60794618818621515 ) ) ;
#2427 = EDGE_CURVE ( 'NONE', #5773, #3865, #480, .T. ) ;
#2428 = EDGE_LOOP ( 'NONE', ( #955, #1026, #4159, #2226, #6103, #1463 ) ) ;
#2429 = FILL_AREA_STYLE_COLOUR ( '', #2454 ) ;
#2430 = AXIS2_PLACEMENT_3D ( 'NONE', #4524, #1655, #4468 ) ;
#2431 = EDGE_LOOP ( 'NONE', ( #4600, #5834, #5599, #2712 ) ) ;
#2432 = FACE_OUTER_BOUND ( 'NONE', #4602, .T. ) ;
#2433 = CARTESIAN_POINT ( 'NONE',  ( 2.941541598353386116E-14, -7.604078429494091299E-14, -35.00000000000000000 ) ) ;
#2434 = DIRECTION ( 'NONE',  ( -0.000000000000000000, -0.000000000000000000, -1.000000000000000000 ) ) ;
#2435 = DIRECTION ( 'NONE',  ( 1.083109739416506025E-19, -7.833442389487322064E-17, -1.000000000000000000 ) ) ;
#2436 = CARTESIAN_POINT ( 'NONE',  ( 8.967351122863068014, -7.487361748921665061, 22.92808036848186504 ) ) ;
#2437 = VECTOR ( 'NONE', #2835, 1000.000000000000000 ) ;
#2438 = AXIS2_PLACEMENT_3D ( 'NONE', #1517, #2048, #1133 ) ;
#2439 = EDGE_CURVE ( 'NONE', #2239, #2261, #852, .T. ) ;
#2440 = EDGE_LOOP ( 'NONE', ( #2524, #1617, #4970, #4165 ) ) ;
#2441 = CARTESIAN_POINT ( 'NONE',  ( -0.9193131588476050053, 11.85339260696609642, 30.72304697887226510 ) ) ;
#2442 = CARTESIAN_POINT ( 'NONE',  ( -12.31015466235523981, 79.04720167209522685, -35.00000000000000000 ) ) ;
#2444 = AXIS2_PLACEMENT_3D ( 'NONE', #2724, #4626, #2757 ) ;
#2443 = DIRECTION ( 'NONE',  ( -0.000000000000000000, -0.000000000000000000, 1.000000000000000000 ) ) ;
#2445 = VERTEX_POINT ( 'NONE', #441 ) ;
#2446 = DIRECTION ( 'NONE',  ( -1.000000000000000000, 0.000000000000000000, 0.000000000000000000 ) ) ;
#2447 = AXIS2_PLACEMENT_3D ( 'NONE', #5062, #3991, #2539 ) ;
#2448 = EDGE_CURVE ( 'NONE', #193, #2445, #937, .T. ) ;
#2449 = LINE ( 'NONE', #4713, #3446 ) ;
#2450 = AXIS2_PLACEMENT_3D ( 'NONE', #5862, #3480, #4953 ) ;
#2451 = CARTESIAN_POINT ( 'NONE',  ( 5.273949241992675674, -14.79903580929012463, 38.00000000000000711 ) ) ;
#2452 =( GEOMETRIC_REPRESENTATION_CONTEXT ( 3 ) GLOBAL_UNCERTAINTY_ASSIGNED_CONTEXT ( ( #3379 ) ) GLOBAL_UNIT_ASSIGNED_CONTEXT ( ( #6056, #5628, #812 ) ) REPRESENTATION_CONTEXT ( 'NONE', 'WORKASPACE' ) );
#2453 = PRODUCT_DEFINITION_CONTEXT ( 'detailed design', #2895, 'design' ) ;
#2454 = COLOUR_RGB ( '',0.7921568627450980005, 0.8196078431372548767, 0.9333333333333333481 ) ;
#2455 = DIRECTION ( 'NONE',  ( 0.9326495259660445569, 0.3607836771741652626, 0.000000000000000000 ) ) ;
#2456 = CARTESIAN_POINT ( 'NONE',  ( -9.692295192624374778, -11.06325188662722248, 38.07291408809469857 ) ) ;
#2457 = ORIENTED_EDGE ( 'NONE', *, *, #6077, .F. ) ;
#2458 = DIRECTION ( 'NONE',  ( 0.000000000000000000, 0.000000000000000000, 1.000000000000000000 ) ) ;
#2459 = CLOSED_SHELL ( 'NONE', ( #5594, #4685, #5213, #3638, #5801, #1015, #3802, #3307, #4856, #5905, #1251, #2885, #1766, #5867, #4770, #5495, #5667, #933, #5738, #3721, #1528, #3465, #5717, #4175, #6058, #4509, #4065, #4709, #3986, #209, #1291, #1701, #3085, #2408, #512, #2286, #2818, #926, #5407, #1599, #4028, #4294, #5300, #4106, #3764, #5751, #1482, #1940, #433, #6087, #612, #3123, #4415, #5449, #3961, #1813, #2508, #1235, #1292, #6099, #5414, #357, #4624, #4715, #5838, #5709, #4344, #1434, #1784, #1059, #4060, #1559, #3345, #5912, #977, #5625, #4488, #3987, #2623, #5598, #3163, #5441, #3223, #426, #1709, #3952, #3095, #4332, #4926, #391, #4169, #2177, #5385, #4710, #3683, #3678, #3877 ) ) ;
#2460 = DIRECTION ( 'NONE',  ( -0.7071067811865573427, 8.659560562355053653E-17, 0.7071067811865378028 ) ) ;
#2461 = CARTESIAN_POINT ( 'NONE',  ( -67.48246767247790956, -25.10212255632935197, 35.00000000000000000 ) ) ;
#2462 = ORIENTED_EDGE ( 'NONE', *, *, #5521, .T. ) ;
#2463 = CYLINDRICAL_SURFACE ( 'NONE', #202, 55.00000000000001421 ) ;
#2464 = CIRCLE ( 'NONE', #5055, 10.00000000000000355 ) ;
#2465 = CARTESIAN_POINT ( 'NONE',  ( 6.563632016262921809, -12.41454131244164216, 35.72510948639917672 ) ) ;
#2466 = ORIENTED_EDGE ( 'NONE', *, *, #5338, .T. ) ;
#2467 = DIRECTION ( 'NONE',  ( -0.000000000000000000, -0.000000000000000000, 1.000000000000000000 ) ) ;
#2468 = VERTEX_POINT ( 'NONE', #4158 ) ;
#2469 = PLANE ( 'NONE',  #302 ) ;
#2470 = CARTESIAN_POINT ( 'NONE',  ( 0.000000000000000000, 12.00000000000000355, -35.00000000000000000 ) ) ;
#2471 = DIRECTION ( 'NONE',  ( -0.000000000000000000, 0.000000000000000000, 1.000000000000000000 ) ) ;
#2472 = CARTESIAN_POINT ( 'NONE',  ( 0.000000000000000000, 0.000000000000000000, 0.000000000000000000 ) ) ;
#2473 = CIRCLE ( 'NONE', #3460, 72.00000000000004263 ) ;
#2474 = CYLINDRICAL_SURFACE ( 'NONE', #3658, 5.000000000000004441 ) ;
#2475 = CARTESIAN_POINT ( 'NONE',  ( 8.963566137365393871, -5.819377809724670669, 22.99383900881164067 ) ) ;
#2476 = VECTOR ( 'NONE', #541, 1000.000000000000000 ) ;
#2477 = AXIS2_PLACEMENT_3D ( 'NONE', #3052, #1557, #5464 ) ;
#2478 = ORIENTED_EDGE ( 'NONE', *, *, #2600, .T. ) ;
#2479 = CARTESIAN_POINT ( 'NONE',  ( 4.807771419025856474, 13.07374771013670767, 35.76776546669863421 ) ) ;
#2480 = ADVANCED_BREP_SHAPE_REPRESENTATION ( '', ( #4196, #73 ), #5734 ) ;
#2481 = VECTOR ( 'NONE', #4935, 1000.000000000000114 ) ;
#2482 = CARTESIAN_POINT ( 'NONE',  ( 9.999999999999998224, 9.999999999999998224, 23.00000000000000000 ) ) ;
#2483 = CARTESIAN_POINT ( 'NONE',  ( -14.67638808697651420, -0.9595328539162122361, 38.18288438803428875 ) ) ;
#2484 = ADVANCED_FACE ( 'NONE', ( #5600 ), #5630, .T. ) ;
#2485 = ORIENTED_EDGE ( 'NONE', *, *, #6093, .F. ) ;
#2486 = CARTESIAN_POINT ( 'NONE',  ( -58.45671475544962448, -33.75000000000001421, -35.00000000000000000 ) ) ;
#2487 = VECTOR ( 'NONE', #4934, 1000.000000000000000 ) ;
#2488 = CARTESIAN_POINT ( 'NONE',  ( -8.963566061094550008, -5.819383256046894992, 22.99383858586043061 ) ) ;
#2489 = VERTEX_POINT ( 'NONE', #4212 ) ;
#2490 = CARTESIAN_POINT ( 'NONE',  ( -9.999999999999998224, -9.999999999999998224, 23.00000000000000000 ) ) ;
#2491 = EDGE_CURVE ( 'NONE', #2502, #4858, #5263, .T. ) ;
#2492 = CARTESIAN_POINT ( 'NONE',  ( 9.618700053625529378, 10.13908112636437231, 30.46372964425718521 ) ) ;
#2493 = CARTESIAN_POINT ( 'NONE',  ( -56.07162667343580864, -45.16605674834639217, 45.00000000000000711 ) ) ;
#2494 = ORIENTED_EDGE ( 'NONE', *, *, #2773, .F. ) ;
#2495 = CARTESIAN_POINT ( 'NONE',  ( 90.08403291566594362, 27.64547812922851833, -79.99999999999998579 ) ) ;
#2496 = DIRECTION ( 'NONE',  ( -0.000000000000000000, -0.000000000000000000, -1.000000000000000000 ) ) ;
#2497 = CARTESIAN_POINT ( 'NONE',  ( -1.594625153350711036E-14, -1.594625153350706303E-14, -20.00000000000000000 ) ) ;
#2498 = EDGE_LOOP ( 'NONE', ( #5681, #2946 ) ) ;
#2499 = CARTESIAN_POINT ( 'NONE',  ( 7.610208295502465248, -9.462636878983104793, 25.48187184588751819 ) ) ;
#2500 = VERTEX_POINT ( 'NONE', #6128 ) ;
#2501 = FILL_AREA_STYLE ('',( #2429 ) ) ;
#2502 = VERTEX_POINT ( 'NONE', #1850 ) ;
#2503 = LINE ( 'NONE', #3980, #4352 ) ;
#2504 = LINE ( 'NONE', #3574, #3562 ) ;
#2505 = DIRECTION ( 'NONE',  ( 3.352022284123619087E-17, 2.150297872858176494E-18, 1.000000000000000000 ) ) ;
#2506 = CARTESIAN_POINT ( 'NONE',  ( -9.557272410707509991, -9.557272410707509991, 28.03893107092312675 ) ) ;
#2507 = DIRECTION ( 'NONE',  ( 0.000000000000000000, 0.000000000000000000, -1.000000000000000000 ) ) ;
#2508 = ADVANCED_FACE ( 'NONE', ( #3200 ), #6070, .F. ) ;
#2509 = ORIENTED_EDGE ( 'NONE', *, *, #5532, .F. ) ;
#2510 = CARTESIAN_POINT ( 'NONE',  ( 4.532931003857846086, 11.42336634021359387, 30.68084270896568810 ) ) ;
#2511 = CARTESIAN_POINT ( 'NONE',  ( -5.273949241992676562, 14.79903580929012286, 38.00000000000000711 ) ) ;
#2512 = DIRECTION ( 'NONE',  ( 1.000000000000000000, 0.000000000000000000, 0.000000000000000000 ) ) ;
#2513 = EDGE_LOOP ( 'NONE', ( #5670, #4265, #4157, #33 ) ) ;
#2514 = DIRECTION ( 'NONE',  ( 1.000000000000000000, 0.000000000000000000, 0.000000000000000000 ) ) ;
#2515 = CARTESIAN_POINT ( 'NONE',  ( -11.22195964661421641, -5.390571672161848404, 30.65936073406735574 ) ) ;
#2516 = EDGE_LOOP ( 'NONE', ( #2178, #4875, #2672, #861, #42 ) ) ;
#2517 = EDGE_CURVE ( 'NONE', #3083, #3081, #5082, .T. ) ;
#2518 = EDGE_CURVE ( 'NONE', #3250, #670, #6096, .T. ) ;
#2519 = CARTESIAN_POINT ( 'NONE',  ( 8.333333333333316162, -9.999999999999998224, 23.00000000000000000 ) ) ;
#2520 = EDGE_CURVE ( 'NONE', #5804, #1288, #389, .T. ) ;
#2521 = CARTESIAN_POINT ( 'NONE',  ( 9.871311131128940985, 2.570253631893256951, 25.61911440830482789 ) ) ;
#2522 = EDGE_CURVE ( 'NONE', #1834, #3364, #3629, .T. ) ;
#2523 = DIRECTION ( 'NONE',  ( -0.000000000000000000, -0.000000000000000000, 1.000000000000000000 ) ) ;
#2524 = ORIENTED_EDGE ( 'NONE', *, *, #1260, .F. ) ;
#2525 = CARTESIAN_POINT ( 'NONE',  ( -27.50000000000000355, -47.63139720814412215, 35.00000000000000000 ) ) ;
#2526 = CARTESIAN_POINT ( 'NONE',  ( -67.92475106770288562, -25.56373185532869741, 35.00000000000000000 ) ) ;
#2527 = CARTESIAN_POINT ( 'NONE',  ( 2.923529524533178936, -13.51119013911330846, 35.79437308157104525 ) ) ;
#2528 = ADVANCED_FACE ( 'NONE', ( #1272, #383 ), #829, .F. ) ;
#2529 = VERTEX_POINT ( 'NONE', #353 ) ;
#2530 = ORIENTED_EDGE ( 'NONE', *, *, #793, .T. ) ;
#2531 = CARTESIAN_POINT ( 'NONE',  ( 13.19705249345142484, 6.492124056756818362, 38.13875458540265129 ) ) ;
#2532 = CARTESIAN_POINT ( 'NONE',  ( 14.99999999999995559, -1.301042606982600272E-14, 20.00000000000000000 ) ) ;
#2533 = CONTEXT_DEPENDENT_SHAPE_REPRESENTATION ( #4280, #3036 ) ;
#2534 = CARTESIAN_POINT ( 'NONE',  ( -8.999999999988011368, -9.000000000000007105, 23.06137295785747909 ) ) ;
#2535 = CARTESIAN_POINT ( 'NONE',  ( 52.58482424179591419, -72.37680137756305498, -79.99999999999998579 ) ) ;
#2536 = ORIENTED_EDGE ( 'NONE', *, *, #2903, .F. ) ;
#2537 = CARTESIAN_POINT ( 'NONE',  ( 80.08403291566592941, 27.64547812922851833, -79.99999999999998579 ) ) ;
#2538 = DIRECTION ( 'NONE',  ( 0.1538769332794418798, -0.9880900209011900248, 0.000000000000000000 ) ) ;
#2539 = DIRECTION ( 'NONE',  ( 1.000000000000000000, 0.000000000000000000, 0.000000000000000000 ) ) ;
#2540 = VECTOR ( 'NONE', #810, 999.9999999999998863 ) ;
#2541 = ORIENTED_EDGE ( 'NONE', *, *, #2788, .F. ) ;
#2542 = DIRECTION ( 'NONE',  ( 1.000000000000000000, 0.000000000000000000, 0.000000000000000000 ) ) ;
#2543 = CARTESIAN_POINT ( 'NONE',  ( -10.85316926984840791, -1.776762854451772622, 28.17414535953233923 ) ) ;
#2544 = ORIENTED_EDGE ( 'NONE', *, *, #4564, .T. ) ;
#2545=STYLED_ITEM('',(#6198),#4196);
#2546 = CARTESIAN_POINT ( 'NONE',  ( -0.8333333333333816650, -9.999999999999998224, 23.00000000000000000 ) ) ;
#2547 = AXIS2_PLACEMENT_3D ( 'NONE', #2394, #3294, #4215 ) ;
#2548 = B_SPLINE_CURVE_WITH_KNOTS ( 'NONE', 3,
 ( #2461, #2526, #2164, #4447 ),
 .UNSPECIFIED., .F., .F.,
 ( 4, 4 ),
 ( 3.469446951953614189E-18, 0.001907370850883722234 ),
 .UNSPECIFIED. ) ;
#2549 = AXIS2_PLACEMENT_3D ( 'NONE', #997, #2880, #1094 ) ;
#2550 = AXIS2_PLACEMENT_3D ( 'NONE', #3738, #3218, #6120 ) ;
#2551 = EDGE_CURVE ( 'NONE', #3749, #2972, #2262, .T. ) ;
#2552 = CARTESIAN_POINT ( 'NONE',  ( 11.79778917763282209, 1.839621235173125369, 30.71783072571432882 ) ) ;
#2553 = CIRCLE ( 'NONE', #4959, 2.499999999999998668 ) ;
#2554 = ORIENTED_EDGE ( 'NONE', *, *, #5378, .T. ) ;
#2555 = DIRECTION ( 'NONE',  ( 0.1538769332794359124, 0.9880900209011910240, 0.000000000000000000 ) ) ;
#2556 = AXIS2_PLACEMENT_3D ( 'NONE', #5101, #2166, #821 ) ;
#2557 = DIRECTION ( 'NONE',  ( -0.000000000000000000, -0.000000000000000000, -1.000000000000000000 ) ) ;
#2558 = EDGE_CURVE ( 'NONE', #3160, #3083, #1981, .T. ) ;
#2559 = DIRECTION ( 'NONE',  ( -0.000000000000000000, -0.000000000000000000, -1.000000000000000000 ) ) ;
#2560 = CARTESIAN_POINT ( 'NONE',  ( -1.016991241531519652, -14.74111653287705792, 38.35393095385146012 ) ) ;
#2561 = ORIENTED_EDGE ( 'NONE', *, *, #4643, .T. ) ;
#2562 = CARTESIAN_POINT ( 'NONE',  ( 74.61196207728410457, -28.86269417393182479, -35.00000000000000000 ) ) ;
#2563 = EDGE_LOOP ( 'NONE', ( #2544, #3778, #5924, #830, #5907, #3430, #3724, #2541, #2509 ) ) ;
#2564 = LINE ( 'NONE', #1084, #6051 ) ;
#2565 = CARTESIAN_POINT ( 'NONE',  ( 85.08403291566592941, 27.64547812922851833, -40.00000000000000000 ) ) ;
#2566 = LINE ( 'NONE', #5843, #2128 ) ;
#2567 = EDGE_CURVE ( 'NONE', #1042, #1017, #2577, .T. ) ;
#2568 = LINE ( 'NONE', #4967, #1577 ) ;
#2569 = VERTEX_POINT ( 'NONE', #3844 ) ;
#2570 = VECTOR ( 'NONE', #2595, 1000.000000000000000 ) ;
#2571 = ORIENTED_EDGE ( 'NONE', *, *, #3951, .F. ) ;
#2572 = CARTESIAN_POINT ( 'NONE',  ( -55.71784976887420271, -21.55374571496209057, -35.00000000000000000 ) ) ;
#2573 = CARTESIAN_POINT ( 'NONE',  ( 13.97471987708211216, -7.178663235509287865, 38.00000000000000000 ) ) ;
#2574 = EDGE_LOOP ( 'NONE', ( #2120, #1872, #2069, #4139 ) ) ;
#2575 = AXIS2_PLACEMENT_3D ( 'NONE', #1739, #3641, #1282 ) ;
#2576 = CARTESIAN_POINT ( 'NONE',  ( -13.77854189090673742, 0.9833031778629290898, 35.81030296219172726 ) ) ;
#2577 = CIRCLE ( 'NONE', #995, 55.00000000000002132 ) ;
#2578 = ORIENTED_EDGE ( 'NONE', *, *, #350, .F. ) ;
#2579 = AXIS2_PLACEMENT_3D ( 'NONE', #2181, #1726, #1244 ) ;
#2580 = CARTESIAN_POINT ( 'NONE',  ( 0.000000000000000000, 0.000000000000000000, -40.00000000000000000 ) ) ;
#2581 = VECTOR ( 'NONE', #981, 1000.000000000000000 ) ;
#2582 = CARTESIAN_POINT ( 'NONE',  ( 10.70751606408959411, 3.531709963121627105, 28.15279306126448944 ) ) ;
#2583 = DIRECTION ( 'NONE',  ( -0.000000000000000000, -0.000000000000000000, 1.000000000000000000 ) ) ;
#2584 = ORIENTED_EDGE ( 'NONE', *, *, #4407, .F. ) ;
#2585 = CARTESIAN_POINT ( 'NONE',  ( 57.35713647666955950, -46.20154318182373032, -35.00000000000000000 ) ) ;
#2586 =( REPRESENTATION_RELATIONSHIP ('NONE','NONE', #4716, #82 ) REPRESENTATION_RELATIONSHIP_WITH_TRANSFORMATION ( #4040 )SHAPE_REPRESENTATION_RELATIONSHIP( ) );
#2587 = DIRECTION ( 'NONE',  ( 0.9880900209011910240, -0.1538769332794358846, 0.000000000000000000 ) ) ;
#2588 = CARTESIAN_POINT ( 'NONE',  ( -1.660914622755444991, -8.965240787521260302, 23.08598164463088054 ) ) ;
#2589 = ORIENTED_EDGE ( 'NONE', *, *, #4893, .T. ) ;
#2590 = DIRECTION ( 'NONE',  ( -0.000000000000000000, -0.000000000000000000, -1.000000000000000000 ) ) ;
#2591 = ORIENTED_EDGE ( 'NONE', *, *, #1984, .T. ) ;
#2592 = CARTESIAN_POINT ( 'NONE',  ( 10.37777353962571425, 10.37777353962603044, 38.05103295300744293 ) ) ;
#2593 = EDGE_CURVE ( 'NONE', #1594, #5460, #1454, .T. ) ;
#2594 = EDGE_CURVE ( 'NONE', #251, #2529, #2819, .T. ) ;
#2595 = DIRECTION ( 'NONE',  ( -0.000000000000000000, -0.000000000000000000, 1.000000000000000000 ) ) ;
#2596 = CARTESIAN_POINT ( 'NONE',  ( -6.247143215332724651E-13, -89.46264649666795776, -79.99999999999998579 ) ) ;
#2597 = CARTESIAN_POINT ( 'NONE',  ( 0.000000000000000000, 0.000000000000000000, 40.00000000000000000 ) ) ;
#2598 = ORIENTED_EDGE ( 'NONE', *, *, #4446, .F. ) ;
#2599 = EDGE_LOOP ( 'NONE', ( #4253, #2986, #1143, #1781 ) ) ;
#2600 = EDGE_CURVE ( 'NONE', #5916, #3596, #701, .T. ) ;
#2601 = LINE ( 'NONE', #3962, #870 ) ;
#2602 = CARTESIAN_POINT ( 'NONE',  ( 15.12434353048566749, 4.260267006495017661, 38.00000000000001421 ) ) ;
#2603 = DIRECTION ( 'NONE',  ( 1.000000000000000000, 0.000000000000000000, 0.000000000000000000 ) ) ;
#2604 = VERTEX_POINT ( 'NONE', #5230 ) ;
#2605 = CARTESIAN_POINT ( 'NONE',  ( -46.52501622030217021, -37.47620048660763103, -35.00000000000000000 ) ) ;
#2606 = CARTESIAN_POINT ( 'NONE',  ( -12.45812449473958239, -3.759289558891018679, 33.24069098933199484 ) ) ;
#2607 = ORIENTED_EDGE ( 'NONE', *, *, #708, .F. ) ;
#2608 = EDGE_CURVE ( 'NONE', #1863, #1594, #4151, .T. ) ;
#2609 = DIRECTION ( 'NONE',  ( -0.000000000000000000, -0.000000000000000000, -1.000000000000000000 ) ) ;
#2610 = CARTESIAN_POINT ( 'NONE',  ( 12.74411457810409232, 5.685785403169719032, 35.74643938915853880 ) ) ;
#2611 = LINE ( 'NONE', #5979, #3923 ) ;
#2612 = ORIENTED_EDGE ( 'NONE', *, *, #1089, .F. ) ;
#2613 = ORIENTED_EDGE ( 'NONE', *, *, #409, .F. ) ;
#2614 = B_SPLINE_CURVE_WITH_KNOTS ( 'NONE', 3,
 ( #3774, #1811, #2390, #5194, #5131, #3708, #5690, #3682, #1845, #5102, #908, #846, #437, #2317 ),
 .UNSPECIFIED., .F., .F.,
 ( 4, 2, 2, 2, 2, 2, 4 ),
 ( 8.673617379884035472E-18, 0.002860246893306399221, 0.004290370339959594277, 0.005720493786612789767, 0.008580740679919178146, 0.01001086412657237017, 0.01144098757322556392 ),
 .UNSPECIFIED. ) ;
#2615 = CARTESIAN_POINT ( 'NONE',  ( -4.154433491267528034, -8.963431154120577560, 23.04275521548131778 ) ) ;
#2616 = ORIENTED_EDGE ( 'NONE', *, *, #2600, .F. ) ;
#2617 = CARTESIAN_POINT ( 'NONE',  ( 58.45671475544921947, 33.75000000000068212, 35.00000000000000000 ) ) ;
#2618 = EDGE_LOOP ( 'NONE', ( #516, #2530, #3475, #3498, #3096, #85, #2578, #3782, #54, #4075 ) ) ;
#2619 = LINE ( 'NONE', #5805, #1743 ) ;
#2620 = DIRECTION ( 'NONE',  ( -0.000000000000000000, 0.000000000000000000, 1.000000000000000000 ) ) ;
#2621 = CARTESIAN_POINT ( 'NONE',  ( 27.50000000000000355, 47.63139720814412215, 35.00000000000000000 ) ) ;
#2622 = CARTESIAN_POINT ( 'NONE',  ( 68.69027832784067300, -26.57196568621440491, -35.00000000000000000 ) ) ;
#2623 = ADVANCED_FACE ( 'NONE', ( #1513 ), #3463, .F. ) ;
#2624 = EDGE_LOOP ( 'NONE', ( #2823, #2952, #2424, #1234 ) ) ;
#2625 = CARTESIAN_POINT ( 'NONE',  ( 9.245260337044141963, 9.269614772507654976, 25.40693856330804223 ) ) ;
#2626 = CARTESIAN_POINT ( 'NONE',  ( 9.910574073276151807, -3.317157231508649495, 22.73823205004162418 ) ) ;
#2627 = CARTESIAN_POINT ( 'NONE',  ( 0.000000000000000000, 0.000000000000000000, 38.00000000000000000 ) ) ;
#2628 = ORIENTED_EDGE ( 'NONE', *, *, #4138, .F. ) ;
#2629 = EDGE_CURVE ( 'NONE', #3966, #2204, #5957, .T. ) ;
#2630 = CARTESIAN_POINT ( 'NONE',  ( 46.52501622030442974, -37.47620048660870395, -35.00000000000000000 ) ) ;
#2631 = EDGE_CURVE ( 'NONE', #2705, #5491, #2857, .T. ) ;
#2632 = CARTESIAN_POINT ( 'NONE',  ( -10.23348454756166070, 8.662453428863081228, 30.54531259719474079 ) ) ;
#2633 = ORIENTED_EDGE ( 'NONE', *, *, #1485, .T. ) ;
#2635 = AXIS2_PLACEMENT_3D ( 'NONE', #1508, #1975, #4751 ) ;
#2634 = FACE_BOUND ( 'NONE', #1273, .T. ) ;
#2636 = EDGE_CURVE ( 'NONE', #1013, #2727, #4555, .T. ) ;
#2637 = VECTOR ( 'NONE', #3973, 1000.000000000000114 ) ;
#2638 = AXIS2_PLACEMENT_3D ( 'NONE', #6074, #1702, #2708 ) ;
#2639 = DIRECTION ( 'NONE',  ( 0.000000000000000000, 0.000000000000000000, 1.000000000000000000 ) ) ;
#2640 = ORIENTED_EDGE ( 'NONE', *, *, #1150, .F. ) ;
#2641 = CARTESIAN_POINT ( 'NONE',  ( -7.178663235509282536, 13.97471987708211216, 38.00000000000000000 ) ) ;
#2642 = AXIS2_PLACEMENT_3D ( 'NONE', #5549, #6044, #517 ) ;
#2643 = CARTESIAN_POINT ( 'NONE',  ( 0.9193131588475976779, -11.85339260696609465, 30.72304697887227576 ) ) ;
#2644 = CIRCLE ( 'NONE', #65, 5.000000000000004441 ) ;
#2645 = EDGE_LOOP ( 'NONE', ( #43, #4535 ) ) ;
#2646 = CARTESIAN_POINT ( 'NONE',  ( -45.92560378283290845, 36.99336990414408888, 35.00000000000000000 ) ) ;
#2647 = ORIENTED_EDGE ( 'NONE', *, *, #2551, .T. ) ;
#2648 = PLANE ( 'NONE',  #1367 ) ;
#2649 = LINE ( 'NONE', #1304, #498 ) ;
#2650 = PRODUCT_CONTEXT ( 'NONE', #695, 'mechanical' ) ;
#2651 = DIRECTION ( 'NONE',  ( -1.000000000000000000, 0.000000000000000000, 0.000000000000000000 ) ) ;
#2652 = CARTESIAN_POINT ( 'NONE',  ( -9.999999999999998224, -4.166666666666622554, 23.00000000000000000 ) ) ;
#2653 = VECTOR ( 'NONE', #2321, 1000.000000000000114 ) ;
#2654 = ORIENTED_EDGE ( 'NONE', *, *, #3407, .T. ) ;
#2655 = LINE ( 'NONE', #6107, #195 ) ;
#2656 = CARTESIAN_POINT ( 'NONE',  ( 10.04707028972858929, 9.166555234036119160, 25.36260747786040071 ) ) ;
#2657 = CARTESIAN_POINT ( 'NONE',  ( 13.97471987708211216, 7.178663235509286089, 38.00000000000000000 ) ) ;
#2658 = CARTESIAN_POINT ( 'NONE',  ( -9.500000000000008882, 67.50000000000000000, 20.00000000000000000 ) ) ;
#2659 = EDGE_LOOP ( 'NONE', ( #4184, #2313, #4641, #4438 ) ) ;
#2660 = DIRECTION ( 'NONE',  ( -0.000000000000000000, -0.000000000000000000, -1.000000000000000000 ) ) ;
#2661 = AXIS2_PLACEMENT_3D ( 'NONE', #210, #2055, #1115 ) ;
#2662 = CARTESIAN_POINT ( 'NONE',  ( -13.90087379555095204, 4.954793796408211826, 38.30989703917856559 ) ) ;
#2663 = ORIENTED_EDGE ( 'NONE', *, *, #3710, .F. ) ;
#2664 = DIRECTION ( 'NONE',  ( 1.000000000000000000, 0.000000000000000000, 0.000000000000000000 ) ) ;
#2665 = EDGE_CURVE ( 'NONE', #3865, #5773, #3065, .T. ) ;
#2666 = CIRCLE ( 'NONE', #3843, 15.67638808697555142 ) ;
#2667 = CARTESIAN_POINT ( 'NONE',  ( 6.314393452555577824E-13, -67.50000000000002842, 35.00000000000000000 ) ) ;
#2668 = AXIS2_PLACEMENT_3D ( 'NONE', #643, #4410, #3478 ) ;
#2669 = CARTESIAN_POINT ( 'NONE',  ( -90.08403291566554572, 27.64547812922971914, -40.00000000000000000 ) ) ;
#2670 = AXIS2_PLACEMENT_3D ( 'NONE', #2963, #4931, #3486 ) ;
#2671 = CARTESIAN_POINT ( 'NONE',  ( 0.000000000000000000, 0.000000000000000000, -20.00000000000000000 ) ) ;
#2672 = ORIENTED_EDGE ( 'NONE', *, *, #1415, .F. ) ;
#2673 = EDGE_CURVE ( 'NONE', #5910, #1915, #2748, .T. ) ;
#2674 = VECTOR ( 'NONE', #5648, 1000.000000000000000 ) ;
#2675 = CARTESIAN_POINT ( 'NONE',  ( -4.986905650496099796, -8.963498645742987492, 23.01829711214648455 ) ) ;
#2676 = ORIENTED_EDGE ( 'NONE', *, *, #4466, .F. ) ;
#2677 = DIRECTION ( 'NONE',  ( -1.000000000000000000, 0.000000000000000000, 0.000000000000000000 ) ) ;
#2678 = ORIENTED_EDGE ( 'NONE', *, *, #1810, .F. ) ;
#2679 = FACE_OUTER_BOUND ( 'NONE', #3947, .T. ) ;
#2680 = DIRECTION ( 'NONE',  ( -1.000000000000000000, 0.000000000000000000, 0.000000000000000000 ) ) ;
#2681 = DIRECTION ( 'NONE',  ( 1.000000000000000000, 0.000000000000000000, 0.000000000000000000 ) ) ;
#2682 = CARTESIAN_POINT ( 'NONE',  ( -13.47611570251764768, 8.069545871843430973, 38.00000000000000000 ) ) ;
#2683 = DIRECTION ( 'NONE',  ( 0.3607836771741718684, -0.9326495259660421144, 0.000000000000000000 ) ) ;
#2684 = ORIENTED_EDGE ( 'NONE', *, *, #3752, .F. ) ;
#2685 = CARTESIAN_POINT ( 'NONE',  ( -11.60016251788669450, 72.19966265505019010, 35.04915833130718994 ) ) ;
#2686 = LINE ( 'NONE', #4585, #1335 ) ;
#2687 = SURFACE_STYLE_FILL_AREA ( #811 ) ;
#2688 = ADVANCED_FACE ( 'NONE', ( #1420 ), #1579, .T. ) ;
#2689 = CARTESIAN_POINT ( 'NONE',  ( 11.02055295301484428, -6.248212340465907566, 30.63787875916901626 ) ) ;
#2690 = B_SPLINE_CURVE_WITH_KNOTS ( 'NONE', 3,
 ( #4653, #1753, #1807, #2812 ),
 .UNSPECIFIED., .F., .F.,
 ( 4, 4 ),
 ( 0.000000000000000000, 0.001907370850883695563 ),
 .UNSPECIFIED. ) ;
#2691 = CARTESIAN_POINT ( 'NONE',  ( -9.977717576970368540, 7.732441893382045350, 28.03187055541259909 ) ) ;
#2692 = ORIENTED_EDGE ( 'NONE', *, *, #1450, .F. ) ;
#2693 = CARTESIAN_POINT ( 'NONE',  ( -5.954763795926128367, 9.638809746143360613, 25.54536317066255791 ) ) ;
#2694 = FACE_OUTER_BOUND ( 'NONE', #3560, .T. ) ;
#2695 = DIRECTION ( 'NONE',  ( 0.000000000000000000, -0.000000000000000000, -1.000000000000000000 ) ) ;
#2696 = EDGE_CURVE ( 'NONE', #4711, #2774, #2041, .T. ) ;
#2697 = EDGE_CURVE ( 'NONE', #4858, #1165, #2985, .T. ) ;
#2698 = LINE ( 'NONE', #4594, #5544 ) ;
#2699 = PLANE ( 'NONE',  #763 ) ;
#2700 = ORIENTED_EDGE ( 'NONE', *, *, #635, .F. ) ;
#2701 = EDGE_CURVE ( 'NONE', #5813, #3749, #6076, .T. ) ;
#2702 = CARTESIAN_POINT ( 'NONE',  ( -5.819377809724670669, -8.963566137365395647, 22.99383900881164777 ) ) ;
#2703 = ORIENTED_EDGE ( 'NONE', *, *, #2933, .T. ) ;
#2704 = DIRECTION ( 'NONE',  ( 1.000000000000000000, 0.000000000000000000, 0.000000000000000000 ) ) ;
#2705 = VERTEX_POINT ( 'NONE', #390 ) ;
#2706 = CYLINDRICAL_SURFACE ( 'NONE', #5555, 100.0000000000000000 ) ;
#2707 = CARTESIAN_POINT ( 'NONE',  ( 50.91502622129181788, 15.00000000000000355, 35.00000000000000000 ) ) ;
#2708 = DIRECTION ( 'NONE',  ( 0.5000000000000101030, -0.8660254037844328234, 0.000000000000000000 ) ) ;
#2709 = CARTESIAN_POINT ( 'NONE',  ( -9.930636381741159369, 5.809855716632678302, 22.73823205004162418 ) ) ;
#2710 = EDGE_CURVE ( 'NONE', #1308, #2828, #798, .T. ) ;
#2711 = LINE ( 'NONE', #2271, #1475 ) ;
#2712 = ORIENTED_EDGE ( 'NONE', *, *, #5990, .F. ) ;
#2713 = DIRECTION ( 'NONE',  ( 1.000000000000000000, 0.000000000000000000, 0.000000000000000000 ) ) ;
#2714 = DIRECTION ( 'NONE',  ( -0.000000000000000000, -0.000000000000000000, -1.000000000000000000 ) ) ;
#2715 = CARTESIAN_POINT ( 'NONE',  ( 7.356224370874624441, 12.70872189800938834, 38.12480727770459055 ) ) ;
#2716 = CARTESIAN_POINT ( 'NONE',  ( 12.81596724893641159, 0.9505942623811802772, 33.26667497053200151 ) ) ;
#2717 = CARTESIAN_POINT ( 'NONE',  ( -13.07374771013671122, 4.807771419025852033, 35.76776546669862711 ) ) ;
#2718 = ORIENTED_EDGE ( 'NONE', *, *, #5876, .T. ) ;
#2719 = CARTESIAN_POINT ( 'NONE',  ( -2.830884587392748841, 12.60026679007841288, 33.25110354061416018 ) ) ;
#2720 = DIRECTION ( 'NONE',  ( 1.000000000000000000, 0.000000000000000000, 0.000000000000000000 ) ) ;
#2721 = LINE ( 'NONE', #408, #5933 ) ;
#2722 = DIRECTION ( 'NONE',  ( 0.000000000000000000, 0.000000000000000000, 1.000000000000000000 ) ) ;
#2723 = AXIS2_PLACEMENT_3D ( 'NONE', #4305, #5289, #2387 ) ;
#2724 = CARTESIAN_POINT ( 'NONE',  ( 0.000000000000000000, 0.000000000000000000, 38.99999999999995737 ) ) ;
#2725 = AXIS2_PLACEMENT_3D ( 'NONE', #6015, #3635, #5054 ) ;
#2726 = CARTESIAN_POINT ( 'NONE',  ( -15.67638808697555142, 0.000000000000000000, 205.0000000000000568 ) ) ;
#2727 = VERTEX_POINT ( 'NONE', #5672 ) ;
#2728 = DIRECTION ( 'NONE',  ( -0.000000000000000000, -0.000000000000000000, -1.000000000000000000 ) ) ;
#2729 = AXIS2_PLACEMENT_3D ( 'NONE', #540, #4377, #3445 ) ;
#2730 = ORIENTED_EDGE ( 'NONE', *, *, #4531, .F. ) ;
#2731 = CARTESIAN_POINT ( 'NONE',  ( 11.60016251788720076, -72.19966265505010483, 35.04915833130718994 ) ) ;
#2732 = CIRCLE ( 'NONE', #5234, 81.00000000000004263 ) ;
#2733 = LINE ( 'NONE', #2266, #3741 ) ;
#2734 = EDGE_CURVE ( 'NONE', #4773, #132, #5554, .T. ) ;
#2735 = FACE_OUTER_BOUND ( 'NONE', #1413, .T. ) ;
#2736 = CARTESIAN_POINT ( 'NONE',  ( -15.56315586465742484, 2.164213882025736613, 38.00000000000000711 ) ) ;
#2737 = AXIS2_PLACEMENT_3D ( 'NONE', #2844, #3252, #4201 ) ;
#2738 = VECTOR ( 'NONE', #4018, 1000.000000000000000 ) ;
#2739 = DIRECTION ( 'NONE',  ( 0.9326495259660420034, 0.3607836771741718129, 0.000000000000000000 ) ) ;
#2740 = ORIENTED_EDGE ( 'NONE', *, *, #9, .F. ) ;
#2741 = FACE_OUTER_BOUND ( 'NONE', #5238, .T. ) ;
#2742 = DIRECTION ( 'NONE',  ( 0.000000000000000000, -1.000000000000000000, 0.000000000000000000 ) ) ;
#2743 = EDGE_CURVE ( 'NONE', #2101, #3175, #2711, .T. ) ;
#2744 = CARTESIAN_POINT ( 'NONE',  ( -1.900794651634388321, 14.58443831393954859, 38.18056006088393417 ) ) ;
#2745 = AXIS2_PLACEMENT_3D ( 'NONE', #1050, #2376, #2407 ) ;
#2746 = EDGE_CURVE ( 'NONE', #2529, #3160, #176, .T. ) ;
#2747 = TOROIDAL_SURFACE ( 'NONE', #3834, 5.141101056459331353, 10.00000000000000000 ) ;
#2748 = B_SPLINE_CURVE_WITH_KNOTS ( 'NONE', 3,
 ( #32, #1910, #157, #5860 ),
 .UNSPECIFIED., .F., .F.,
 ( 4, 4 ),
 ( 3.469446951953614189E-18, 0.001907370850886582576 ),
 .UNSPECIFIED. ) ;
#2749 = CARTESIAN_POINT ( 'NONE',  ( 11.85339260696609287, -2.780846643040693260E-14, 30.72304697887226510 ) ) ;
#2750 = CARTESIAN_POINT ( 'NONE',  ( -12.11088206474084750, 8.328520801854340405, 38.20782360758020957 ) ) ;
#2751 = ORIENTED_EDGE ( 'NONE', *, *, #1222, .F. ) ;
#2752 = CARTESIAN_POINT ( 'NONE',  ( -8.926329112024045997, 11.12736491637288339, 35.63514765224430647 ) ) ;
#2753 = DIRECTION ( 'NONE',  ( 1.000000000000000000, 0.000000000000000000, 0.000000000000000000 ) ) ;
#2754 = ORIENTED_EDGE ( 'NONE', *, *, #1984, .F. ) ;
#2755 = DIRECTION ( 'NONE',  ( -0.000000000000000000, -0.000000000000000000, -1.000000000000000000 ) ) ;
#2756 = VECTOR ( 'NONE', #2182, 1000.000000000000000 ) ;
#2757 = DIRECTION ( 'NONE',  ( 1.000000000000000000, 0.000000000000000000, 0.000000000000000000 ) ) ;
#2758 = CIRCLE ( 'NONE', #501, 5.000000000000004441 ) ;
#2759 = EDGE_CURVE ( 'NONE', #1920, #915, #2258, .T. ) ;
#2760 = AXIS2_PLACEMENT_3D ( 'NONE', #1921, #1464, #552 ) ;
#2761 = CARTESIAN_POINT ( 'NONE',  ( -6.925743867604849946, -10.16167434176052176, 28.06532504456334820 ) ) ;
#2762 = ORIENTED_EDGE ( 'NONE', *, *, #723, .T. ) ;
#2763 = DIRECTION ( 'NONE',  ( -0.000000000000000000, -0.000000000000000000, 1.000000000000000000 ) ) ;
#2764 = VECTOR ( 'NONE', #1486, 1000.000000000000000 ) ;
#2765 = EDGE_LOOP ( 'NONE', ( #549, #4663, #2999, #713 ) ) ;
#2766 = CARTESIAN_POINT ( 'NONE',  ( -12.50000000000155431, 67.50000000000002842, 35.00000000000000000 ) ) ;
#2767 = DIRECTION ( 'NONE',  ( -0.000000000000000000, -0.000000000000000000, -1.000000000000000000 ) ) ;
#2768 = ORIENTED_EDGE ( 'NONE', *, *, #5007, .T. ) ;
#2769 = CARTESIAN_POINT ( 'NONE',  ( -14.79903580929011930, -5.273949241992674786, 38.00000000000000000 ) ) ;
#2770 = VECTOR ( 'NONE', #4010, 1000.000000000000000 ) ;
#2771 = CARTESIAN_POINT ( 'NONE',  ( -12.50000000000155431, 67.50000000000002842, -35.00000000000000000 ) ) ;
#2772 = ADVANCED_FACE ( 'NONE', ( #2800, #5113 ), #5175, .T. ) ;
#2773 = EDGE_CURVE ( 'NONE', #5376, #1649, #2553, .T. ) ;
#2774 = VERTEX_POINT ( 'NONE', #1397 ) ;
#2775 = FACE_OUTER_BOUND ( 'NONE', #2618, .T. ) ;
#2776 = CARTESIAN_POINT ( 'NONE',  ( 12.49999999999999822, 67.50000000000000000, -19.00000000000000711 ) ) ;
#2777 = CARTESIAN_POINT ( 'NONE',  ( -4.709709529607297718, 13.90855959397112862, 38.16103891068026144 ) ) ;
#2778 = APPLICATION_CONTEXT ( 'automotive_design' ) ;
#2779 = CARTESIAN_POINT ( 'NONE',  ( 8.965240827029074211, 1.660911000355770328, 23.08598180255751942 ) ) ;
#2780 = EDGE_CURVE ( 'NONE', #3800, #1013, #1965, .T. ) ;
#2781 = EDGE_CURVE ( 'NONE', #3309, #2774, #4048, .T. ) ;
#2782 = CARTESIAN_POINT ( 'NONE',  ( 0.000000000000000000, 0.000000000000000000, 45.00000000000000711 ) ) ;
#2783 = ORIENTED_EDGE ( 'NONE', *, *, #2397, .T. ) ;
#2784 = CARTESIAN_POINT ( 'NONE',  ( -7.487361748921619764, 8.967351122863068014, 22.92808036848186504 ) ) ;
#2785 = FACE_OUTER_BOUND ( 'NONE', #4067, .T. ) ;
#2786 = ORIENTED_EDGE ( 'NONE', *, *, #5150, .T. ) ;
#2787 = FACE_OUTER_BOUND ( 'NONE', #2428, .T. ) ;
#2788 = EDGE_CURVE ( 'NONE', #4001, #2218, #1573, .T. ) ;
#2789 = CARTESIAN_POINT ( 'NONE',  ( -11.02058084744346544, -6.248091806769219048, 30.63788045528724524 ) ) ;
#2790 = DIRECTION ( 'NONE',  ( -1.000000000000000000, 0.000000000000000000, 0.000000000000000000 ) ) ;
#2791 = CARTESIAN_POINT ( 'NONE',  ( -7.869812776064898152, -10.50531938289192979, 30.57803900350706883 ) ) ;
#2792 = ORIENTED_EDGE ( 'NONE', *, *, #1051, .T. ) ;
#2793 = DIRECTION ( 'NONE',  ( 1.000000000000000000, 0.000000000000000000, 0.000000000000000000 ) ) ;
#2794 = ORIENTED_EDGE ( 'NONE', *, *, #4408, .T. ) ;
#2795 = DIRECTION ( 'NONE',  ( 0.000000000000000000, 0.000000000000000000, 1.000000000000000000 ) ) ;
#2796 = DIRECTION ( 'NONE',  ( -1.000000000000000000, 0.000000000000000000, 0.000000000000000000 ) ) ;
#2797 = CARTESIAN_POINT ( 'NONE',  ( 12.00000000000000000, 12.00000000000000355, 20.00000000000000000 ) ) ;
#2798 = ORIENTED_EDGE ( 'NONE', *, *, #99, .F. ) ;
#2799 = CARTESIAN_POINT ( 'NONE',  ( 0.000000000000000000, 89.46264649666795776, 40.00000000000000000 ) ) ;
#2800 = FACE_BOUND ( 'NONE', #678, .T. ) ;
#2801 = EDGE_LOOP ( 'NONE', ( #4632, #3688, #4240, #5147, #1226, #842, #1764, #5222, #2740 ) ) ;
#2802 = ORIENTED_EDGE ( 'NONE', *, *, #3706, .T. ) ;
#2803 = FACE_OUTER_BOUND ( 'NONE', #4809, .T. ) ;
#2804 = DIRECTION ( 'NONE',  ( 1.000000000000000000, 0.000000000000000000, 0.000000000000000000 ) ) ;
#2805 = CARTESIAN_POINT ( 'NONE',  ( 0.9766276285328842066, 14.65181115585160931, 38.18271774125523876 ) ) ;
#2806 = DIRECTION ( 'NONE',  ( -0.000000000000000000, -0.000000000000000000, -1.000000000000000000 ) ) ;
#2807 = EDGE_CURVE ( 'NONE', #5943, #3250, #4223, .T. ) ;
#2808 = PLANE ( 'NONE',  #1969 ) ;
#2809 = ORIENTED_EDGE ( 'NONE', *, *, #5211, .F. ) ;
#2810 = CARTESIAN_POINT ( 'NONE',  ( -4.273103006804785053, 9.778265433844637755, 25.59105575288735324 ) ) ;
#2811 = VERTEX_POINT ( 'NONE', #6137 ) ;
#2812 = CARTESIAN_POINT ( 'NONE',  ( -11.33314185116896589, -72.77350886803867525, 35.13717928826270054 ) ) ;
#2813 = EDGE_CURVE ( 'NONE', #3566, #4690, #3239, .T. ) ;
#2814 = ORIENTED_EDGE ( 'NONE', *, *, #5103, .T. ) ;
#2815 = CARTESIAN_POINT ( 'NONE',  ( 0.000000000000000000, 0.000000000000000000, 205.0000000000000568 ) ) ;
#2816 = CARTESIAN_POINT ( 'NONE',  ( 15.00000000000000178, 52.91502622129183209, 35.00000000000000000 ) ) ;
#2817 = CARTESIAN_POINT ( 'NONE',  ( 0.000000000000000000, 0.000000000000000000, -35.00000000000000000 ) ) ;
#2818 = ADVANCED_FACE ( 'NONE', ( #1822 ), #1307, .F. ) ;
#2819 = B_SPLINE_CURVE_WITH_KNOTS ( 'NONE', 3,
 ( #2951, #2456, #3353, #1008, #4311, #3319, #1882, #1035, #64, #2010, #5725, #5693, #2887, #131, #3807, #1949, #5822, #515, #973, #3777, #4789, #5763, #1488, #542, #4347, #4863 ),
 .UNSPECIFIED., .F., .F.,
 ( 4, 2, 2, 2, 2, 2, 2, 2, 2, 2, 2, 2, 4 ),
 ( 2.453269466693398698E-18, 0.002857484983890242261, 0.004286227475835359922, 0.005714969967780478451, 0.008572454951670712905, 0.01000119744361583143, 0.01142993993556095170, 0.01428742491945118875, 0.01571616741139630902, 0.01714490990334142928, 0.02000239488723166634, 0.02143113737917678660, 0.02285987987112190686 ),
 .UNSPECIFIED. ) ;
#2820 = CARTESIAN_POINT ( 'NONE',  ( 9.933255351449997050, 9.419333092093003401, 30.50691708577705796 ) ) ;
#2821 = ORIENTED_EDGE ( 'NONE', *, *, #2788, .T. ) ;
#2822 = DIRECTION ( 'NONE',  ( 0.7787725926866119197, -0.6273063437270283149, 0.000000000000000000 ) ) ;
#2823 = ORIENTED_EDGE ( 'NONE', *, *, #5766, .T. ) ;
#2824 = PLANE ( 'NONE',  #3234 ) ;
#2825 = PLANE ( 'NONE',  #5154 ) ;
#2826 = CIRCLE ( 'NONE', #6018, 4.999999999999990230 ) ;
#2827 = SURFACE_STYLE_FILL_AREA ( #1362 ) ;
#2828 = VERTEX_POINT ( 'NONE', #4640 ) ;
#2829 = CARTESIAN_POINT ( 'NONE',  ( -8.056095891487838412E-14, 1.254589464284425060E-14, -35.00000000000000000 ) ) ;
#2830 = CARTESIAN_POINT ( 'NONE',  ( 4.986905650496026077, -8.963498645742987492, 23.01829711214648455 ) ) ;
#2831 = AXIS2_PLACEMENT_3D ( 'NONE', #318, #2220, #4980 ) ;
#2832 = ORIENTED_EDGE ( 'NONE', *, *, #5676, .T. ) ;
#2833 = ORIENTED_EDGE ( 'NONE', *, *, #3236, .F. ) ;
#2834 = CARTESIAN_POINT ( 'NONE',  ( 0.000000000000000000, 0.000000000000000000, -35.00000000000000000 ) ) ;
#2835 = DIRECTION ( 'NONE',  ( -0.000000000000000000, -0.000000000000000000, 1.000000000000000000 ) ) ;
#2836 = LINE ( 'NONE', #1466, #893 ) ;
#2837 = DIRECTION ( 'NONE',  ( 0.000000000000000000, 0.000000000000000000, 1.000000000000000000 ) ) ;
#2838 = LINE ( 'NONE', #1406, #2073 ) ;
#2839 = CARTESIAN_POINT ( 'NONE',  ( 12.64059746256322470, -7.570044180282070378, 38.23931193745811186 ) ) ;
#2840 = CIRCLE ( 'NONE', #2549, 12.49999999999999822 ) ;
#2841 = VERTEX_POINT ( 'NONE', #2771 ) ;
#2842 = CARTESIAN_POINT ( 'NONE',  ( 2.491918585145488585, 8.964680801521355491, 23.07363600708416129 ) ) ;
#2843 = CARTESIAN_POINT ( 'NONE',  ( 1.082228759108216032, 15.67638808697554786, 38.00000000000000711 ) ) ;
#2844 = CARTESIAN_POINT ( 'NONE',  ( -85.08403291566612836, -27.64547812922793923, -79.99999999999998579 ) ) ;
#2845 = PRODUCT ( 'Stationary spindle', 'Stationary spindle', '', ( #3575 ) ) ;
#2846 = VERTEX_POINT ( 'NONE', #335 ) ;
#2847 = CARTESIAN_POINT ( 'NONE',  ( 74.61196207728339402, 28.86269417393366865, 35.00000000000000000 ) ) ;
#2848 = AXIS2_PLACEMENT_3D ( 'NONE', #5743, #4878, #4838 ) ;
#2849=STYLED_ITEM('',(#6170),#2153);
#2850 = CARTESIAN_POINT ( 'NONE',  ( 68.69027832784067300, -26.57196568621440491, 35.13717928826310555 ) ) ;
#2851 = EDGE_CURVE ( 'NONE', #2186, #2998, #2758, .T. ) ;
#2852 = EDGE_CURVE ( 'NONE', #2204, #3836, #1334, .T. ) ;
#2853 = DIRECTION ( 'NONE',  ( 0.000000000000000000, 1.000000000000000000, -0.000000000000000000 ) ) ;
#2854 = CARTESIAN_POINT ( 'NONE',  ( -6.000548030722248072, -9.000000000000003553, 23.13502304888920591 ) ) ;
#2855 = AXIS2_PLACEMENT_3D ( 'NONE', #423, #1253, #4642 ) ;
#2856 = ADVANCED_FACE ( 'NONE', ( #5146 ), #3135, .F. ) ;
#2857 = LINE ( 'NONE', #3448, #1100 ) ;
#2858 = ORIENTED_EDGE ( 'NONE', *, *, #3786, .F. ) ;
#2859 = LINE ( 'NONE', #4257, #866 ) ;
#2860 = CARTESIAN_POINT ( 'NONE',  ( -10.54244016040621013, 10.54244016040621013, 30.50000000000000000 ) ) ;
#2861 = AXIS2_PLACEMENT_3D ( 'NONE', #1675, #3111, #5602 ) ;
#2862 = DIRECTION ( 'NONE',  ( 1.000000000000000000, 0.000000000000000000, 0.000000000000000000 ) ) ;
#2863 = ORIENTED_EDGE ( 'NONE', *, *, #4845, .F. ) ;
#2864 = CARTESIAN_POINT ( 'NONE',  ( 14.67638808697506292, -0.4806947631990224901, 38.18288438803429585 ) ) ;
#2865 = VECTOR ( 'NONE', #1280, 1000.000000000000000 ) ;
#2866 = CARTESIAN_POINT ( 'NONE',  ( 3.645499761006324224, -11.58282027941459269, 30.69674202529824569 ) ) ;
#2867 = ORIENTED_EDGE ( 'NONE', *, *, #2558, .F. ) ;
#2868 = VERTEX_POINT ( 'NONE', #1355 ) ;
#2869 = CARTESIAN_POINT ( 'NONE',  ( 9.192833548570215285, 59.02994620157096506, 35.00000000000000000 ) ) ;
#2870 = DIRECTION ( 'NONE',  ( -0.000000000000000000, -0.000000000000000000, 1.000000000000000000 ) ) ;
#2871 = CARTESIAN_POINT ( 'NONE',  ( 52.91502622129182498, 15.00000000000001954, 35.00000000000000000 ) ) ;
#2872 =( NAMED_UNIT ( * ) SI_UNIT ( $, .STERADIAN. ) SOLID_ANGLE_UNIT ( ) );
#2873 = AXIS2_PLACEMENT_3D ( 'NONE', #3298, #1396, #3325 ) ;
#2874 = CARTESIAN_POINT ( 'NONE',  ( -9.074396217167327805, 58.26942451214400620, 35.00000000000000000 ) ) ;
#2875 = DIRECTION ( 'NONE',  ( 0.7787725926866080339, 0.6273063437270329779, 0.000000000000000000 ) ) ;
#2876 = AXIS2_PLACEMENT_3D ( 'NONE', #5013, #5282, #1501 ) ;
#2877 = EDGE_LOOP ( 'NONE', ( #5038, #1363, #4418, #5329, #5489, #5064 ) ) ;
#2878 = CARTESIAN_POINT ( 'NONE',  ( 6.400535080091637852, 11.71455171164206988, 33.18278799730942552 ) ) ;
#2879 = CARTESIAN_POINT ( 'NONE',  ( 5.833333333333365900, 9.999999999999998224, 23.00000000000000000 ) ) ;
#2880 = DIRECTION ( 'NONE',  ( 0.000000000000000000, 0.000000000000000000, -1.000000000000000000 ) ) ;
#2881 = EDGE_LOOP ( 'NONE', ( #1792, #4913, #4429, #4442 ) ) ;
#2882 = CARTESIAN_POINT ( 'NONE',  ( 4.130675435985391572E-14, 1.067806758184284836E-13, -35.00000000000000000 ) ) ;
#2883 = CARTESIAN_POINT ( 'NONE',  ( -11.39256393965315439, -7.228764404800518406, 33.15620429642044087 ) ) ;
#2884 = FACE_OUTER_BOUND ( 'NONE', #2053, .T. ) ;
#2885 = ADVANCED_FACE ( 'NONE', ( #4689 ), #1365, .T. ) ;
#2886 = CARTESIAN_POINT ( 'NONE',  ( -10.37777353962637505, 10.37777353962536608, 38.05103295300745003 ) ) ;
#2887 = CARTESIAN_POINT ( 'NONE',  ( -0.4914066504967060656, -14.67601930163249513, 38.18288424882399568 ) ) ;
#2888 = ORIENTED_EDGE ( 'NONE', *, *, #5471, .T. ) ;
#2889 = CARTESIAN_POINT ( 'NONE',  ( 100.0000000000000000, 1.224646799147353217E-14, -39.00000000000002842 ) ) ;
#2890 = DIRECTION ( 'NONE',  ( -0.7071067811865464625, 0.7071067811865486830, 0.000000000000000000 ) ) ;
#2891 = VERTEX_POINT ( 'NONE', #4209 ) ;
#2892 = EDGE_CURVE ( 'NONE', #3029, #4172, #1695, .T. ) ;
#2893 = CARTESIAN_POINT ( 'NONE',  ( 11.06391443747510195, -9.691632641776605439, 38.07293523736169760 ) ) ;
#2894 = CARTESIAN_POINT ( 'NONE',  ( 7.570233152424892253, -12.64046943599297101, 38.23931941266578605 ) ) ;
#2895 = APPLICATION_CONTEXT ( 'automotive_design' ) ;
#2896 = ORIENTED_EDGE ( 'NONE', *, *, #5448, .F. ) ;
#2897 = SURFACE_SIDE_STYLE ('',( #1343 ) ) ;
#2898 = ORIENTED_EDGE ( 'NONE', *, *, #3427, .T. ) ;
#2899 = CARTESIAN_POINT ( 'NONE',  ( 0.000000000000000000, 0.000000000000000000, 35.00000000000000000 ) ) ;
#2900 = CARTESIAN_POINT ( 'NONE',  ( -52.58482424179536707, 72.37680137756343868, -79.99999999999998579 ) ) ;
#2901 = CARTESIAN_POINT ( 'NONE',  ( 0.000000000000000000, 0.000000000000000000, 0.000000000000000000 ) ) ;
#2902 = CARTESIAN_POINT ( 'NONE',  ( 90.08403291566575888, -27.64547812922912939, 40.00000000000000000 ) ) ;
#2903 = EDGE_CURVE ( 'NONE', #670, #5794, #201, .T. ) ;
#2904 = DIRECTION ( 'NONE',  ( 0.000000000000000000, -0.000000000000000000, -1.000000000000000000 ) ) ;
#2905 = ORIENTED_EDGE ( 'NONE', *, *, #1669, .F. ) ;
#2906 = CARTESIAN_POINT ( 'NONE',  ( 1.776706711792238824, 10.85317354580219451, 28.17414650202874427 ) ) ;
#2907 = CARTESIAN_POINT ( 'NONE',  ( 3.333333333333376558, 9.999999999999998224, 23.00000000000000000 ) ) ;
#2908 = CARTESIAN_POINT ( 'NONE',  ( -14.67638808697555319, 1.484446970801598990E-11, 38.18288438803429585 ) ) ;
#2909 = ORIENTED_EDGE ( 'NONE', *, *, #5338, .F. ) ;
#2910 = CARTESIAN_POINT ( 'NONE',  ( 27.60043906316099083, 27.60043906316109386, 35.00000000000000000 ) ) ;
#2911 = CARTESIAN_POINT ( 'NONE',  ( -8.964415603276487232, -6.652779355836718089, 22.96342386064221941 ) ) ;
#2912 = CARTESIAN_POINT ( 'NONE',  ( 7.178663235509283425, -13.97471987708211572, 38.00000000000000000 ) ) ;
#2913 = CARTESIAN_POINT ( 'NONE',  ( 0.000000000000000000, 67.50000000000000000, -19.00000000000000000 ) ) ;
#2914 = DIRECTION ( 'NONE',  ( 1.000000000000000000, 0.000000000000000000, -0.000000000000000000 ) ) ;
#2915 = ORIENTED_EDGE ( 'NONE', *, *, #5502, .T. ) ;
#2916 = CARTESIAN_POINT ( 'NONE',  ( -54.99999999999990052, -21.27605460800010206, 35.00000000000000000 ) ) ;
#2917 = CARTESIAN_POINT ( 'NONE',  ( -57.35713647666923976, 46.20154318182412112, 35.00000000000000000 ) ) ;
#2918 = ORIENTED_EDGE ( 'NONE', *, *, #4180, .T. ) ;
#2919 = FACE_BOUND ( 'NONE', #3187, .T. ) ;
#2920 = CARTESIAN_POINT ( 'NONE',  ( 8.159736356077644359, -11.57174281757876599, 35.66679457777021156 ) ) ;
#2921 = ORIENTED_EDGE ( 'NONE', *, *, #3607, .T. ) ;
#2922 = CARTESIAN_POINT ( 'NONE',  ( -9.618700053625529378, 10.13908112636436520, 30.46372964425718521 ) ) ;
#2923 = AXIS2_PLACEMENT_3D ( 'NONE', #222, #2157, #4051 ) ;
#2924 = ORIENTED_EDGE ( 'NONE', *, *, #3415, .T. ) ;
#2925 = CARTESIAN_POINT ( 'NONE',  ( 55.48030965893076427, -45.89047003626308197, 35.00000000000000000 ) ) ;
#2926 = EDGE_CURVE ( 'NONE', #1883, #4004, #1299, .T. ) ;
#2927 = CYLINDRICAL_SURFACE ( 'NONE', #5031, 4.999999999999997335 ) ;
#2928 = CARTESIAN_POINT ( 'NONE',  ( -100.0000000000000000, 0.000000000000000000, 40.00000000000000000 ) ) ;
#2929 = DIRECTION ( 'NONE',  ( -0.7358482210391271705, 0.6771465096960568308, 0.000000000000000000 ) ) ;
#2930 = DIRECTION ( 'NONE',  ( 1.000000000000000000, 1.776356839400250465E-15, 0.000000000000000000 ) ) ;
#2931 = CARTESIAN_POINT ( 'NONE',  ( 10.67320828294309543, -8.785766938566929696, 33.09220912812762805 ) ) ;
#2932 = AXIS2_PLACEMENT_3D ( 'NONE', #3114, #5552, #855 ) ;
#2933 = EDGE_CURVE ( 'NONE', #464, #6095, #5104, .T. ) ;
#2934 = ORIENTED_EDGE ( 'NONE', *, *, #1625, .F. ) ;
#2935 = EDGE_CURVE ( 'NONE', #1194, #1606, #2165, .T. ) ;
#2936 = CARTESIAN_POINT ( 'NONE',  ( -0.8581648076837100625, 9.928243323025455425, 25.63579099555274965 ) ) ;
#2937 = CARTESIAN_POINT ( 'NONE',  ( 3.317157231508649495, 9.910574073276151807, 22.73823205004162418 ) ) ;
#2939 = AXIS2_PLACEMENT_3D ( 'NONE', #786, #5040, #4499 ) ;
#2938 = CARTESIAN_POINT ( 'NONE',  ( -27.50000000000010303, 47.63139720814406530, 35.00000000000000000 ) ) ;
#2940 = AXIS2_PLACEMENT_3D ( 'NONE', #124, #5352, #2004 ) ;
#2941 = ORIENTED_EDGE ( 'NONE', *, *, #2746, .T. ) ;
#2942 = LINE ( 'NONE', #603, #4528 ) ;
#2943 = CIRCLE ( 'NONE', #1344, 80.99999999999998579 ) ;
#2944 = AXIS2_PLACEMENT_3D ( 'NONE', #5384, #781, #3932 ) ;
#2945 = CARTESIAN_POINT ( 'NONE',  ( -11.79779776130985702, 1.839547822007354894, 30.71783115363461647 ) ) ;
#2946 = ORIENTED_EDGE ( 'NONE', *, *, #1266, .T. ) ;
#2947 = CARTESIAN_POINT ( 'NONE',  ( -5.833333333333365900, -9.999999999999998224, 23.00000000000000000 ) ) ;
#2948 = AXIS2_PLACEMENT_3D ( 'NONE', #1500, #46, #5840 ) ;
#2949 = AXIS2_PLACEMENT_3D ( 'NONE', #3544, #4506, #4541 ) ;
#2950 = LINE ( 'NONE', #1070, #3169 ) ;
#2951 = CARTESIAN_POINT ( 'NONE',  ( -10.37777353962477278, -10.37777353962696303, 38.05103295300743582 ) ) ;
#2952 = ORIENTED_EDGE ( 'NONE', *, *, #5708, .F. ) ;
#2953 = DIRECTION ( 'NONE',  ( -0.000000000000000000, -0.000000000000000000, 1.000000000000000000 ) ) ;
#2954 = CARTESIAN_POINT ( 'NONE',  ( 0.000000000000000000, 0.000000000000000000, 35.00000000000000000 ) ) ;
#2955 = PRODUCT_DEFINITION ( 'UNKNOWN', '', #1842, #1321 ) ;
#2956 = DIRECTION ( 'NONE',  ( -1.000000000000000000, 0.000000000000000000, 0.000000000000000000 ) ) ;
#2957 = ORIENTED_EDGE ( 'NONE', *, *, #4383, .T. ) ;
#2958 = VECTOR ( 'NONE', #4675, 1000.000000000000000 ) ;
#2959 = CARTESIAN_POINT ( 'NONE',  ( 10.27356722921338594, -10.12138240269939082, 35.55812462721154787 ) ) ;
#2960 = ORIENTED_EDGE ( 'NONE', *, *, #4239, .F. ) ;
#2961 = DIRECTION ( 'NONE',  ( -0.000000000000000000, -0.000000000000000000, -1.000000000000000000 ) ) ;
#2962 = ORIENTED_EDGE ( 'NONE', *, *, #2743, .F. ) ;
#2963 = CARTESIAN_POINT ( 'NONE',  ( 0.000000000000000000, 0.000000000000000000, -35.00000000000000000 ) ) ;
#2964 = CARTESIAN_POINT ( 'NONE',  ( -6.247143215332724651E-13, -89.46264649666795776, -40.00000000000000000 ) ) ;
#2965 = AXIS2_PLACEMENT_3D ( 'NONE', #5085, #6100, #5988 ) ;
#2966 = DIRECTION ( 'NONE',  ( -1.000000000000000000, 0.000000000000000000, 0.000000000000000000 ) ) ;
#2967 = DIRECTION ( 'NONE',  ( 1.000000000000000000, 0.000000000000000000, 0.000000000000000000 ) ) ;
#2968 = CIRCLE ( 'NONE', #3368, 5.141101056459331353 ) ;
#2969 = EDGE_CURVE ( 'NONE', #5798, #2297, #1919, .T. ) ;
#2970 = EDGE_CURVE ( 'NONE', #5318, #3527, #2968, .T. ) ;
#2971 = AXIS2_PLACEMENT_3D ( 'NONE', #1892, #79, #3759 ) ;
#2972 = VERTEX_POINT ( 'NONE', #3806 ) ;
#2973 = CARTESIAN_POINT ( 'NONE',  ( 2.334726591726390495E-14, 11.85339260696609465, 30.72304697887226510 ) ) ;
#2974 = CIRCLE ( 'NONE', #5865, 12.50000000000000178 ) ;
#2975 = CARTESIAN_POINT ( 'NONE',  ( 14.99999999999995559, -1.301042606982600272E-14, -20.00000000000000000 ) ) ;
#2976 = CARTESIAN_POINT ( 'NONE',  ( 11.33314185116896589, 72.77350886803867525, 35.13717928826270054 ) ) ;
#2977 = ORIENTED_EDGE ( 'NONE', *, *, #2396, .T. ) ;
#2978 = EDGE_CURVE ( 'NONE', #4044, #1046, #5470, .T. ) ;
#2979 = AXIS2_PLACEMENT_3D ( 'NONE', #454, #530, #5745 ) ;
#2980 = CARTESIAN_POINT ( 'NONE',  ( -8.964680801521355491, -2.491918585145397991, 23.07363600708416129 ) ) ;
#2981 = ORIENTED_EDGE ( 'NONE', *, *, #3761, .F. ) ;
#2982 = CARTESIAN_POINT ( 'NONE',  ( 6.642184745761413822, -9.939337621248920840, 22.73823205004162773 ) ) ;
#2983 = EDGE_CURVE ( 'NONE', #4283, #656, #5663, .T. ) ;
#2984 = CARTESIAN_POINT ( 'NONE',  ( 11.69030472852370650, 2.742560498089724685, 30.70728637550628903 ) ) ;
#2985 = LINE ( 'NONE', #4895, #4351 ) ;
#2986 = ORIENTED_EDGE ( 'NONE', *, *, #5982, .F. ) ;
#2987 = CARTESIAN_POINT ( 'NONE',  ( -80.08403291566554572, 27.64547812922971914, -79.99999999999998579 ) ) ;
#2988 = CYLINDRICAL_SURFACE ( 'NONE', #3930, 12.50000000000139089 ) ;
#2989 = FACE_OUTER_BOUND ( 'NONE', #4502, .T. ) ;
#2990 = CARTESIAN_POINT ( 'NONE',  ( -4.954793796408214490, -13.90087379555094493, 38.30989703917857270 ) ) ;
#2991 = EDGE_LOOP ( 'NONE', ( #1101, #6069 ) ) ;
#2992 = EDGE_LOOP ( 'NONE', ( #1597, #5836, #5687, #3359 ) ) ;
#2993 = DIRECTION ( 'NONE',  ( 0.9326495259660518844, -0.3607836771741464998, 0.000000000000000000 ) ) ;
#2994 = CARTESIAN_POINT ( 'NONE',  ( -58.45671475544946816, -33.75000000000027711, 35.00000000000000000 ) ) ;
#2995 = CONTEXT_DEPENDENT_SHAPE_REPRESENTATION ( #1418, #61 ) ;
#2996 = DIRECTION ( 'NONE',  ( -1.000000000000000000, 0.000000000000000000, 0.000000000000000000 ) ) ;
#2997 = FACE_OUTER_BOUND ( 'NONE', #4188, .T. ) ;
#2998 = VERTEX_POINT ( 'NONE', #5293 ) ;
#2999 = ORIENTED_EDGE ( 'NONE', *, *, #1869, .T. ) ;
#3000 = LINE ( 'NONE', #5847, #4514 ) ;
#3001 = CARTESIAN_POINT ( 'NONE',  ( 9.916251082295017838, 4.147343260682109900, 22.73823205004162418 ) ) ;
#3002 = DIRECTION ( 'NONE',  ( 1.000000000000000000, 0.000000000000000000, 0.000000000000000000 ) ) ;
#3003 = EDGE_CURVE ( 'NONE', #4984, #2020, #1007, .T. ) ;
#3004 = EDGE_LOOP ( 'NONE', ( #3016, #1621 ) ) ;
#3005 = CARTESIAN_POINT ( 'NONE',  ( 9.074396217167732814, -58.26942451214393515, 35.00000000000000000 ) ) ;
#3006 = CARTESIAN_POINT ( 'NONE',  ( -14.42236408824967064, -3.019346778933471143, 38.33740271606986028 ) ) ;
#3007 = ORIENTED_EDGE ( 'NONE', *, *, #2813, .T. ) ;
#3008 = CARTESIAN_POINT ( 'NONE',  ( -10.43169748385511042, -11.73806315776973541, 38.00000000000000711 ) ) ;
#3009 = EDGE_CURVE ( 'NONE', #5996, #3996, #2356, .T. ) ;
#3010 = CARTESIAN_POINT ( 'NONE',  ( 12.41454131244163506, 6.563632016262926250, 35.72510948639917672 ) ) ;
#3011 = EDGE_LOOP ( 'NONE', ( #2194, #3284, #5472, #5789, #256 ) ) ;
#3012 = LINE ( 'NONE', #2495, #3240 ) ;
#3013 = EDGE_CURVE ( 'NONE', #1611, #3081, #2950, .T. ) ;
#3014 = CARTESIAN_POINT ( 'NONE',  ( -9.192833548570002122, 59.02994620156853500, 35.00000000000000000 ) ) ;
#3015 = CARTESIAN_POINT ( 'NONE',  ( -4.399209358691967608, -10.59950146047779818, 28.13666863833443799 ) ) ;
#3016 = ORIENTED_EDGE ( 'NONE', *, *, #2608, .F. ) ;
#3017 = DIRECTION ( 'NONE',  ( -0.7071067811865493491, 0.000000000000000000, -0.7071067811865456854 ) ) ;
#3018 = ORIENTED_EDGE ( 'NONE', *, *, #5759, .F. ) ;
#3019 = CARTESIAN_POINT ( 'NONE',  ( 13.74495680931392450, 5.167291852657578843, 38.15579506865712034 ) ) ;
#3020 = CARTESIAN_POINT ( 'NONE',  ( 57.35713647666955950, -46.20154318182373032, 35.00000000000000000 ) ) ;
#3021 = APPLICATION_PROTOCOL_DEFINITION ( 'draft international standard', 'automotive_design', 1998, #695 ) ;
#3022 = LINE ( 'NONE', #1645, #1336 ) ;
#3023 = CARTESIAN_POINT ( 'NONE',  ( 55.71784976887403928, 21.55374571496248137, 35.00000000000000000 ) ) ;
#3024 = ORIENTED_EDGE ( 'NONE', *, *, #5184, .T. ) ;
#3025 = LINE ( 'NONE', #2537, #4205 ) ;
#3026 = CARTESIAN_POINT ( 'NONE',  ( 90.08403291566594362, 27.64547812922851833, 40.00000000000000000 ) ) ;
#3027 = CARTESIAN_POINT ( 'NONE',  ( 0.000000000000000000, 0.000000000000000000, -35.00000000000000000 ) ) ;
#3028 = AXIS2_PLACEMENT_3D ( 'NONE', #1894, #3790, #3042 ) ;
#3029 = VERTEX_POINT ( 'NONE', #5195 ) ;
#3030 = EDGE_CURVE ( 'NONE', #5498, #3338, #3409, .T. ) ;
#3031 = CARTESIAN_POINT ( 'NONE',  ( -11.33314185116896589, -72.77350886803867525, 35.13717928826270054 ) ) ;
#3032 = CARTESIAN_POINT ( 'NONE',  ( -11.85339260696609287, 2.318493676985545998E-14, 30.72304697887226510 ) ) ;
#3033 = AXIS2_PLACEMENT_3D ( 'NONE', #2257, #4154, #878 ) ;
#3034 = ORIENTED_EDGE ( 'NONE', *, *, #4992, .T. ) ;
#3035 = DIRECTION ( 'NONE',  ( -0.3607836771741531612, -0.9326495259660493309, 0.000000000000000000 ) ) ;
#3036 = PRODUCT_DEFINITION_SHAPE ( 'NONE', 'NONE',  #6147 ) ;
#3037 = VECTOR ( 'NONE', #3770, 999.9999999999998863 ) ;
#3038 = AXIS2_PLACEMENT_3D ( 'NONE', #3801, #5316, #1062 ) ;
#3039 = EDGE_CURVE ( 'NONE', #4467, #3160, #2389, .T. ) ;
#3040 = EDGE_CURVE ( 'NONE', #1013, #4784, #4252, .T. ) ;
#3041 = CARTESIAN_POINT ( 'NONE',  ( 12.60026679007841288, 2.830884587392749285, 33.25110354061416018 ) ) ;
#3042 = DIRECTION ( 'NONE',  ( -1.000000000000000000, 0.000000000000000000, 0.000000000000000000 ) ) ;
#3043 = ORIENTED_EDGE ( 'NONE', *, *, #4844, .T. ) ;
#3044 = CARTESIAN_POINT ( 'NONE',  ( 62.30180741492923602, -50.18450749816189216, 38.99999999999995737 ) ) ;
#3045 = AXIS2_PLACEMENT_3D ( 'NONE', #5168, #5665, #6042 ) ;
#3046 = CARTESIAN_POINT ( 'NONE',  ( 10.54244016040621190, 10.54244016040621013, 30.50000000000000000 ) ) ;
#3047 = EDGE_CURVE ( 'NONE', #4773, #5881, #1104, .T. ) ;
#3048 = CARTESIAN_POINT ( 'NONE',  ( -0.8581648076837764538, -9.928243323025448319, 25.63579099555280294 ) ) ;
#3049 = ORIENTED_EDGE ( 'NONE', *, *, #1558, .F. ) ;
#3050 = DIRECTION ( 'NONE',  ( -0.000000000000000000, -0.000000000000000000, -1.000000000000000000 ) ) ;
#3051 = VERTEX_POINT ( 'NONE', #3776 ) ;
#3052 = CARTESIAN_POINT ( 'NONE',  ( 0.000000000000000000, -67.50000000000000000, -35.00000000000000000 ) ) ;
#3053 = DIRECTION ( 'NONE',  ( 1.000000000000000000, 0.000000000000000000, 0.000000000000000000 ) ) ;
#3054 = ITEM_DEFINED_TRANSFORMATION ( 'NONE', 'NONE', #1552,  #73 ) ;
#3055 = DIRECTION ( 'NONE',  ( -0.000000000000000000, -0.000000000000000000, -1.000000000000000000 ) ) ;
#3056 = VECTOR ( 'NONE', #922, 1000.000000000000000 ) ;
#3057 = B_SPLINE_CURVE_WITH_KNOTS ( 'NONE', 3,
 ( #3484, #797, #3571, #1610 ),
 .UNSPECIFIED., .F., .F.,
 ( 4, 4 ),
 ( 0.000000000000000000, 0.001907370850883704887 ),
 .UNSPECIFIED. ) ;
#3058 = DIRECTION ( 'NONE',  ( 0.000000000000000000, 0.000000000000000000, 1.000000000000000000 ) ) ;
#3059 = ORIENTED_EDGE ( 'NONE', *, *, #3039, .F. ) ;
#3060 = VECTOR ( 'NONE', #4728, 1000.000000000000000 ) ;
#3061 = ORIENTED_EDGE ( 'NONE', *, *, #5708, .T. ) ;
#3062 = CARTESIAN_POINT ( 'NONE',  ( 8.926511697459378780, 11.12726264164139600, 35.63515070857870626 ) ) ;
#3063 = CARTESIAN_POINT ( 'NONE',  ( 9.969668718019493170, -9.144590365090033757, 22.73823205004162418 ) ) ;
#3064 =( NAMED_UNIT ( * ) SI_UNIT ( $, .STERADIAN. ) SOLID_ANGLE_UNIT ( ) );
#3065 = CIRCLE ( 'NONE', #2068, 5.000000000000004441 ) ;
#3066 = ORIENTED_EDGE ( 'NONE', *, *, #2701, .F. ) ;
#3067 = CYLINDRICAL_SURFACE ( 'NONE', #53, 5.000000000000003553 ) ;
#3068 = CIRCLE ( 'NONE', #197, 12.50000000000000000 ) ;
#3069 = CARTESIAN_POINT ( 'NONE',  ( -14.63234267792704735, 2.035630462091347237, 38.34842398122203377 ) ) ;
#3070 = AXIS2_PLACEMENT_3D ( 'NONE', #3815, #5733, #1955 ) ;
#3071 = EDGE_LOOP ( 'NONE', ( #3301, #5846, #4481, #4397 ) ) ;
#3072 = CYLINDRICAL_SURFACE ( 'NONE', #2038, 12.49999999999999822 ) ;
#3073 = CIRCLE ( 'NONE', #3857, 12.50000000000138733 ) ;
#3074 = VECTOR ( 'NONE', #3106, 1000.000000000000000 ) ;
#3075 = CARTESIAN_POINT ( 'NONE',  ( 9.370308598635419983, 8.432782529159778662, 25.44727941985334496 ) ) ;
#3076 = DIRECTION ( 'NONE',  ( 1.000000000000000000, 0.000000000000000000, 0.000000000000000000 ) ) ;
#3077 = ORIENTED_EDGE ( 'NONE', *, *, #668, .T. ) ;
#3078 = ORIENTED_EDGE ( 'NONE', *, *, #6077, .T. ) ;
#3079 = ADVANCED_FACE ( 'NONE', ( #4861 ), #5538, .F. ) ;
#3080 = CARTESIAN_POINT ( 'NONE',  ( -2.491918585145488585, -8.964680801521357267, 23.07363600708416840 ) ) ;
#3081 = VERTEX_POINT ( 'NONE', #1997 ) ;
#3082 = DIRECTION ( 'NONE',  ( -0.000000000000000000, -0.000000000000000000, -1.000000000000000000 ) ) ;
#3083 = VERTEX_POINT ( 'NONE', #1470 ) ;
#3084 = CARTESIAN_POINT ( 'NONE',  ( -57.58482424179535997, 72.37680137756343868, 40.00000000000000000 ) ) ;
#3085 = ADVANCED_FACE ( 'NONE', ( #5250 ), #4271, .F. ) ;
#3086 = CARTESIAN_POINT ( 'NONE',  ( -68.69027832784050247, 26.57196568621489163, -35.00000000000000000 ) ) ;
#3087 = SHAPE_DEFINITION_REPRESENTATION ( #1895, #4975 ) ;
#3088 = EDGE_CURVE ( 'NONE', #962, #5318, #2377, .T. ) ;
#3089 = CARTESIAN_POINT ( 'NONE',  ( 0.000000000000000000, 0.000000000000000000, 40.00000000000000000 ) ) ;
#3090 = DIRECTION ( 'NONE',  ( -1.000000000000000000, 0.000000000000000000, 0.000000000000000000 ) ) ;
#3091 = ORIENTED_EDGE ( 'NONE', *, *, #3874, .F. ) ;
#3092 = CARTESIAN_POINT ( 'NONE',  ( 8.432825516645548802, 9.370308891928093686, 25.44727539999419719 ) ) ;
#3093 = CARTESIAN_POINT ( 'NONE',  ( 8.586443133426902668E-15, -8.586443133426886890E-15, -20.00000000000000000 ) ) ;
#3094 = PLANE ( 'NONE',  #577 ) ;
#3095 = ADVANCED_FACE ( 'NONE', ( #5680 ), #4232, .F. ) ;
#3096 = ORIENTED_EDGE ( 'NONE', *, *, #4794, .T. ) ;
#3097 = FACE_OUTER_BOUND ( 'NONE', #415, .T. ) ;
#3098 = CARTESIAN_POINT ( 'NONE',  ( -11.58116666691846852, 9.086997423426605991, 38.17633527770230017 ) ) ;
#3099 =( REPRESENTATION_RELATIONSHIP ('NONE','NONE', #4716, #2176 ) REPRESENTATION_RELATIONSHIP_WITH_TRANSFORMATION ( #739 )SHAPE_REPRESENTATION_RELATIONSHIP( ) );
#3100 = VERTEX_POINT ( 'NONE', #558 ) ;
#3101 = DIRECTION ( 'NONE',  ( 1.000000000000000000, 0.000000000000000000, 0.000000000000000000 ) ) ;
#3102 = CARTESIAN_POINT ( 'NONE',  ( 8.970286642449650572, 8.321944142006520551, 22.89273687632151066 ) ) ;
#3103 = DIRECTION ( 'NONE',  ( -0.000000000000000000, -0.000000000000000000, -1.000000000000000000 ) ) ;
#3104 = ORIENTED_EDGE ( 'NONE', *, *, #3615, .F. ) ;
#3105 = CARTESIAN_POINT ( 'NONE',  ( -6.642184745761413822, 9.939337621248920840, 22.73823205004162418 ) ) ;
#3106 = DIRECTION ( 'NONE',  ( -1.000000000000000000, -0.000000000000000000, -0.000000000000000000 ) ) ;
#3107 = CARTESIAN_POINT ( 'NONE',  ( -1.902388932222473850, -12.74242197681752486, 33.26151580524049223 ) ) ;
#3108 = ORIENTED_EDGE ( 'NONE', *, *, #1155, .T. ) ;
#3109 = CYLINDRICAL_SURFACE ( 'NONE', #283, 12.49999999999999645 ) ;
#3110 = EDGE_LOOP ( 'NONE', ( #912, #2962, #1400, #4291, #2403 ) ) ;
#3111 = DIRECTION ( 'NONE',  ( 0.7071067811865482389, -0.7071067811865469066, 0.000000000000000000 ) ) ;
#3112 = LINE ( 'NONE', #1676, #4860 ) ;
#3113 = ITEM_DEFINED_TRANSFORMATION ( 'NONE', 'NONE', #4740,  #73 ) ;
#3114 = CARTESIAN_POINT ( 'NONE',  ( -6.247143215332724651E-13, -89.46264649666795776, -79.99999999999998579 ) ) ;
#3115 = CARTESIAN_POINT ( 'NONE',  ( 12.00000000000000000, 50.91502622129181788, 20.00000000000000000 ) ) ;
#3116 = ADVANCED_FACE ( 'NONE', ( #5283 ), #2808, .F. ) ;
#3117 = ORIENTED_EDGE ( 'NONE', *, *, #3994, .T. ) ;
#3118 = CARTESIAN_POINT ( 'NONE',  ( -62.30180741492890206, 50.18450749816231848, 38.99999999999995737 ) ) ;
#3119 = CARTESIAN_POINT ( 'NONE',  ( 8.785766938566926143, 10.67320828294310076, 33.09220912812762094 ) ) ;
#3120 = CARTESIAN_POINT ( 'NONE',  ( -11.07913919611982223, 71.14248150488573685, 45.00000000000000711 ) ) ;
#3121 = DIRECTION ( 'NONE',  ( -1.000000000000000000, 0.000000000000000000, 0.000000000000000000 ) ) ;
#3122 = ORIENTED_EDGE ( 'NONE', *, *, #3088, .T. ) ;
#3123 = ADVANCED_FACE ( 'NONE', ( #1435 ), #5214, .F. ) ;
#3124 = CARTESIAN_POINT ( 'NONE',  ( -13.11522978513662885, 6.737147714782517838, 38.26633100282688815 ) ) ;
#3125 = EDGE_LOOP ( 'NONE', ( #3701, #1840, #3122, #4969 ) ) ;
#3126 = CARTESIAN_POINT ( 'NONE',  ( 55.00000000000024158, -21.27605460799916770, 35.00000000000000000 ) ) ;
#3128 = CIRCLE ( 'NONE', #1330, 5.000000000000004441 ) ;
#3127 = FACE_BOUND ( 'NONE', #1808, .T. ) ;
#3129 =( LENGTH_UNIT ( ) NAMED_UNIT ( * ) SI_UNIT ( .MILLI., .METRE. ) );
#3130 = B_SPLINE_CURVE_WITH_KNOTS ( 'NONE', 3,
 ( #4443, #617, #200, #5890 ),
 .UNSPECIFIED., .F., .F.,
 ( 4, 4 ),
 ( 0.000000000000000000, 0.001907370850883699249 ),
 .UNSPECIFIED. ) ;
#3131 = VECTOR ( 'NONE', #4267, 1000.000000000000227 ) ;
#3132 = LINE ( 'NONE', #5593, #4026 ) ;
#3133 = CARTESIAN_POINT ( 'NONE',  ( 9.999999999999998224, -9.999999999999998224, -167.0000000000000284 ) ) ;
#3134 = ORIENTED_EDGE ( 'NONE', *, *, #4145, .T. ) ;
#3135 = B_SPLINE_SURFACE_WITH_KNOTS ( 'NONE', 3, 3, ( 
 ( #3816, #2959, #5832, #3390, #1917, #1956, #5275 ),
 ( #4829, #5735, #1461, #4798, #5331, #523, #3362 ),
 ( #3912, #2018, #1553, #3853, #5204, #944, #3884 ),
 ( #137, #2920, #2369, #4290, #4356, #2499, #5802 ),
 ( #2894, #1016, #5771, #586, #109, #1493, #1521 ),
 ( #5302, #2465, #3419, #4771, #5700, #39, #1079 ),
 ( #1044, #1989, #486, #4872, #621, #4388, #2830 ),
 ( #548, #4733, #1889, #4263, #3784, #5241, #14 ),
 ( #1427, #3326, #983, #2866, #2401, #2426, #4319 ),
 ( #74, #2527, #294, #647, #4986, #2137, #4539 ),
 ( #3569, #5420, #3482, #4417, #2175, #1111, #5983 ),
 ( #168, #1636, #4956, #2643, #203, #2049, #5892 ),
 ( #4449, #711, #4066, #1134, #1584, #3946, #1160 ),
 ( #2560, #1191, #4034, #1608, #5488, #3048, #5953 ),
 ( #3506, #1216, #3107, #2077, #3541, #3976, #2588 ),
 ( #1671, #4899, #3454, #4478, #5459, #5014, #3080 ),
 ( #231, #2103, #760, #4925, #4003, #5920, #5368 ),
 ( #2990, #733, #5866, #5394, #3015, #676, #2615 ),
 ( #4504, #259, #2260, #5545, #1324, #5512, #2675 ),
 ( #325, #1789, #3685, #3136, #5047, #5080, #2702 ),
 ( #3626, #5166, #795, #3711, #2761, #3261, #4662 ),
 ( #3226, #1240, #4572, #2791, #5597, #2201, #826 ),
 ( #909, #412, #6006, #5573, #351, #4156, #5134 ),
 ( #4630, #2289, #4092, #380, #879, #4181, #1270 ),
 ( #4599, #6094, #2225, #6068, #1812, #1720, #5627 ) ),
 .UNSPECIFIED., .F., .F., .F.,
 ( 4, 3, 3, 3, 3, 3, 3, 3, 4 ),
 ( 4, 3, 4 ),
 ( 0.000000000000000000, 0.1250000000000000000, 0.2500000000000000000, 0.3750000000000000000, 0.5000000000000000000, 0.6250000000000000000, 0.7500000000000000000, 0.8750000000000000000, 1.000000000000000000 ),
 ( 0.000000000000000000, 0.5087255983319457497, 1.017451196663891499 ),
 .UNSPECIFIED. ) ;
#3136 = CARTESIAN_POINT ( 'NONE',  ( -6.248212340465907566, -11.02055295301484428, 30.63787875916901626 ) ) ;
#3137 = VECTOR ( 'NONE', #3152, 1000.000000000000000 ) ;
#3138 = ORIENTED_EDGE ( 'NONE', *, *, #2759, .T. ) ;
#3139 = PLANE ( 'NONE',  #2949 ) ;
#3140 = ORIENTED_EDGE ( 'NONE', *, *, #4248, .F. ) ;
#3141 = DIRECTION ( 'NONE',  ( 0.000000000000000000, 0.000000000000000000, 1.000000000000000000 ) ) ;
#3142 = CARTESIAN_POINT ( 'NONE',  ( -9.999999999999998224, -9.999999999999998224, -167.0000000000000284 ) ) ;
#3143 = ITEM_DEFINED_TRANSFORMATION ( 'NONE', 'NONE', #1168,  #73 ) ;
#3144 = AXIS2_PLACEMENT_3D ( 'NONE', #3919, #594, #556 ) ;
#3145 = LINE ( 'NONE', #3205, #960 ) ;
#3146 = CARTESIAN_POINT ( 'NONE',  ( -9.999999999999998224, -3.333333333333286408, 23.00000000000000000 ) ) ;
#3147 = CIRCLE ( 'NONE', #5633, 9.500000000000005329 ) ;
#3148 = ORIENTED_EDGE ( 'NONE', *, *, #848, .T. ) ;
#3149 = DIRECTION ( 'NONE',  ( -0.9880900209011901358, -0.1538769332794418798, 0.000000000000000000 ) ) ;
#3150 = CARTESIAN_POINT ( 'NONE',  ( -67.48246767247790956, -25.10212255632935197, 35.00000000000000000 ) ) ;
#3151 = LINE ( 'NONE', #5778, #4153 ) ;
#3152 = DIRECTION ( 'NONE',  ( -0.8660254037844385966, 0.5000000000000001110, 0.000000000000000000 ) ) ;
#3153 = VECTOR ( 'NONE', #1093, 1000.000000000000000 ) ;
#3154 = ADVANCED_FACE ( 'NONE', ( #3337 ), #4561, .T. ) ;
#3155 = EDGE_CURVE ( 'NONE', #1077, #3262, #2112, .T. ) ;
#3156 = ORIENTED_EDGE ( 'NONE', *, *, #5799, .F. ) ;
#3157 = CARTESIAN_POINT ( 'NONE',  ( 8.965668681055126044, -0.8304760625349946190, 23.09216300389308074 ) ) ;
#3158=STYLED_ITEM('',(#6170),#249);
#3159 = CARTESIAN_POINT ( 'NONE',  ( -8.964680801521355491, 2.491918585145488141, 23.07363600708416129 ) ) ;
#3160 = VERTEX_POINT ( 'NONE', #4011 ) ;
#3161 = LINE ( 'NONE', #3530, #2338 ) ;
#3162 = VECTOR ( 'NONE', #4932, 1000.000000000000000 ) ;
#3163 = ADVANCED_FACE ( 'NONE', ( #3514 ), #4255, .T. ) ;
#3164 = PLANE ( 'NONE',  #170 ) ;
#3165 = AXIS2_PLACEMENT_3D ( 'NONE', #4671, #2683, #2739 ) ;
#3166 = AXIS2_PLACEMENT_3D ( 'NONE', #4103, #6020, #3670 ) ;
#3167 = CARTESIAN_POINT ( 'NONE',  ( 4.130675435985391572E-14, 1.067806758184284836E-13, 35.00000000000000000 ) ) ;
#3168 = ORIENTED_EDGE ( 'NONE', *, *, #2108, .F. ) ;
#3169 = VECTOR ( 'NONE', #1881, 1000.000000000000000 ) ;
#3170 = EDGE_CURVE ( 'NONE', #1681, #5243, #1201, .T. ) ;
#3171 = CIRCLE ( 'NONE', #2979, 10.00000000000000178 ) ;
#3172 = CARTESIAN_POINT ( 'NONE',  ( -0.000000000000000000, 50.91502622129181788, -20.00000000000000000 ) ) ;
#3173 = VERTEX_POINT ( 'NONE', #4459 ) ;
#3174 = DIRECTION ( 'NONE',  ( -0.000000000000000000, 0.000000000000000000, 1.000000000000000000 ) ) ;
#3175 = VERTEX_POINT ( 'NONE', #2622 ) ;
#3176 = DIRECTION ( 'NONE',  ( -0.000000000000000000, -0.000000000000000000, -1.000000000000000000 ) ) ;
#3177 = CARTESIAN_POINT ( 'NONE',  ( 0.000000000000000000, -67.50000000000000000, 35.00000000000000000 ) ) ;
#3178 = LINE ( 'NONE', #1731, #2231 ) ;
#3179 = DIRECTION ( 'NONE',  ( -1.000000000000000000, 8.673617379883998001E-16, 0.000000000000000000 ) ) ;
#3180 = CARTESIAN_POINT ( 'NONE',  ( -11.33314185116896589, -72.77350886803867525, 35.00000000000000000 ) ) ;
#3181 = ORIENTED_EDGE ( 'NONE', *, *, #1893, .F. ) ;
#3182 = DIRECTION ( 'NONE',  ( 0.000000000000000000, 0.000000000000000000, 1.000000000000000000 ) ) ;
#3183 = CARTESIAN_POINT ( 'NONE',  ( -12.49999999999999822, -67.50000000000000000, 35.00000000000000000 ) ) ;
#3184 = CARTESIAN_POINT ( 'NONE',  ( -10.03503361918909143, 10.72051346006269235, 38.06197354439402147 ) ) ;
#3185 = CARTESIAN_POINT ( 'NONE',  ( 14.74111653287705792, -5.477421655106639269E-15, 38.35393095385146012 ) ) ;
#3186 = CARTESIAN_POINT ( 'NONE',  ( -12.45811160333930623, 3.759380242563082675, 33.24069127598783524 ) ) ;
#3187 = EDGE_LOOP ( 'NONE', ( #2678, #1082 ) ) ;
#3188 = CARTESIAN_POINT ( 'NONE',  ( -2.923529524533181601, 13.51119013911330846, 35.79437308157104525 ) ) ;
#3189 = EDGE_CURVE ( 'NONE', #464, #1950, #5764, .T. ) ;
#3190 = DIRECTION ( 'NONE',  ( 0.000000000000000000, 0.000000000000000000, 1.000000000000000000 ) ) ;
#3191 = PRODUCT_DEFINITION_SHAPE ( 'NONE', 'NONE',  #118 ) ;
#3192 = DIRECTION ( 'NONE',  ( -0.1538769332794358846, -0.9880900209011910240, 0.000000000000000000 ) ) ;
#3193 = CARTESIAN_POINT ( 'NONE',  ( -55.71784976887214924, 21.55374571496067304, 35.00000000000000000 ) ) ;
#3194 = EDGE_CURVE ( 'NONE', #2828, #1308, #4054, .T. ) ;
#3195 = CARTESIAN_POINT ( 'NONE',  ( 52.58482424179643289, 72.37680137756268550, -79.99999999999998579 ) ) ;
#3196 = UNCERTAINTY_MEASURE_WITH_UNIT (LENGTH_MEASURE( 1.000000000000000082E-05 ), #3129, 'distance_accuracy_value', 'NONE');
#3197 = DIRECTION ( 'NONE',  ( -0.000000000000000000, -0.000000000000000000, -1.000000000000000000 ) ) ;
#3198 = EDGE_CURVE ( 'NONE', #5202, #37, #2085, .T. ) ;
#3199 = ORIENTED_EDGE ( 'NONE', *, *, #5532, .T. ) ;
#3200 = FACE_OUTER_BOUND ( 'NONE', #1124, .T. ) ;
#3201 = ORIENTED_EDGE ( 'NONE', *, *, #350, .T. ) ;
#3202 = DIRECTION ( 'NONE',  ( -1.000000000000000000, 0.000000000000000000, 0.000000000000000000 ) ) ;
#3203 = CARTESIAN_POINT ( 'NONE',  ( 50.91502622129181788, 12.00000000000000355, 35.00000000000000000 ) ) ;
#3204 = ITEM_DEFINED_TRANSFORMATION ( 'NONE', 'NONE', #2848,  #73 ) ;
#3205 = CARTESIAN_POINT ( 'NONE',  ( -1.131281550719566266E-13, -1.761763928569765259E-14, 35.00000000000000000 ) ) ;
#3206 = CARTESIAN_POINT ( 'NONE',  ( 5.114554293134526134E-14, 6.349488965209711204E-14, 35.00000000000000000 ) ) ;
#3207 = DIRECTION ( 'NONE',  ( -1.000000000000000000, 0.000000000000000000, 0.000000000000000000 ) ) ;
#3208 = ORIENTED_EDGE ( 'NONE', *, *, #822, .F. ) ;
#3209 = CARTESIAN_POINT ( 'NONE',  ( 11.08488032081242025, -11.08488032081242203, 38.00000000000000711 ) ) ;
#3210 = CARTESIAN_POINT ( 'NONE',  ( -46.52501622030417394, 37.47620048660903080, 35.00000000000000000 ) ) ;
#3211 = FACE_OUTER_BOUND ( 'NONE', #2349, .T. ) ;
#3212 =( REPRESENTATION_RELATIONSHIP ('NONE','NONE', #4716, #2176 ) REPRESENTATION_RELATIONSHIP_WITH_TRANSFORMATION ( #1247 )SHAPE_REPRESENTATION_RELATIONSHIP( ) );
#3213 = CARTESIAN_POINT ( 'NONE',  ( 14.21238549857230815, -4.003063095775586611, 38.32638145091770809 ) ) ;
#3214 = CARTESIAN_POINT ( 'NONE',  ( -10.16167434176051465, 6.925743867604855275, 28.06532504456334465 ) ) ;
#3215 = EDGE_LOOP ( 'NONE', ( #4128, #450, #5530, #240, #4109, #5631 ) ) ;
#3216 = CARTESIAN_POINT ( 'NONE',  ( -6.787634061845148281, 9.554965159330777169, 25.51646427192168431 ) ) ;
#3217 = CARTESIAN_POINT ( 'NONE',  ( 0.000000000000000000, 0.000000000000000000, 40.00000000000000000 ) ) ;
#3218 = DIRECTION ( 'NONE',  ( 0.000000000000000000, 0.000000000000000000, 1.000000000000000000 ) ) ;
#3219 = DIRECTION ( 'NONE',  ( -0.7071067811865524577, 0.000000000000000000, -0.7071067811865426878 ) ) ;
#3220 = CIRCLE ( 'NONE', #566, 5.141101056459331353 ) ;
#3221 = LINE ( 'NONE', #1384, #6121 ) ;
#3222 = AXIS2_PLACEMENT_3D ( 'NONE', #5091, #5060, #1740 ) ;
#3223 = ADVANCED_FACE ( 'NONE', ( #4997 ), #1170, .F. ) ;
#3224 = VECTOR ( 'NONE', #5298, 1000.000000000000000 ) ;
#3225 = ADVANCED_FACE ( 'NONE', ( #5963 ), #686, .T. ) ;
#3226 = CARTESIAN_POINT ( 'NONE',  ( -8.328520801854340405, -12.11088206474084927, 38.20782360758020246 ) ) ;
#3227 = ORIENTED_EDGE ( 'NONE', *, *, #2352, .T. ) ;
#3228 = CARTESIAN_POINT ( 'NONE',  ( 0.000000000000000000, 0.000000000000000000, -35.00000000000000000 ) ) ;
#3229 = AXIS2_PLACEMENT_3D ( 'NONE', #4307, #60, #98 ) ;
#3230 = ORIENTED_EDGE ( 'NONE', *, *, #21, .T. ) ;
#3231 = FACE_OUTER_BOUND ( 'NONE', #5403, .T. ) ;
#3232 = CIRCLE ( 'NONE', #4831, 12.50000000000138556 ) ;
#3233 = CARTESIAN_POINT ( 'NONE',  ( -80.99999999999998579, 0.000000000000000000, -40.00000000000000000 ) ) ;
#3234 = AXIS2_PLACEMENT_3D ( 'NONE', #1884, #4185, #1852 ) ;
#3235 = FACE_OUTER_BOUND ( 'NONE', #2574, .T. ) ;
#3236 = EDGE_CURVE ( 'NONE', #4835, #2202, #508, .T. ) ;
#3237 = CARTESIAN_POINT ( 'NONE',  ( -13.97471987708211216, 7.178663235509287865, 38.00000000000000711 ) ) ;
#3238 = CONICAL_SURFACE ( 'NONE', #4433, 80.00000000000000000, 0.7853981633974482790 ) ;
#3239 = LINE ( 'NONE', #1860, #5863 ) ;
#3240 = VECTOR ( 'NONE', #4002, 1000.000000000000000 ) ;
#3241 = ORIENTED_EDGE ( 'NONE', *, *, #3189, .F. ) ;
#3242 = DIRECTION ( 'NONE',  ( -0.9880900209011901358, -0.1538769332794418798, 0.000000000000000000 ) ) ;
#3243 = CARTESIAN_POINT ( 'NONE',  ( -1.630640067418198669E-13, 67.50000000000002842, -35.00000000000000000 ) ) ;
#3244 = DIRECTION ( 'NONE',  ( 0.9326495259660445569, 0.3607836771741652626, 0.000000000000000000 ) ) ;
#3245 = CARTESIAN_POINT ( 'NONE',  ( -8.007183658747742072, 11.03292118881348394, 33.12420745160152791 ) ) ;
#3246 = AXIS2_PLACEMENT_3D ( 'NONE', #4088, #321, #6003 ) ;
#3247 = EDGE_CURVE ( 'NONE', #5574, #1077, #4463, .T. ) ;
#3248 = CARTESIAN_POINT ( 'NONE',  ( 10.59950146047779462, -4.399209358691971161, 28.13666863833444154 ) ) ;
#3249 = FILL_AREA_STYLE_COLOUR ( '', #1554 ) ;
#3250 = VERTEX_POINT ( 'NONE', #2149 ) ;
#3251 = CARTESIAN_POINT ( 'NONE',  ( -3.878911688431554428, 13.33506331686138147, 35.78373290693656372 ) ) ;
#3252 = DIRECTION ( 'NONE',  ( -0.000000000000000000, -0.000000000000000000, 1.000000000000000000 ) ) ;
#3253 = ORIENTED_EDGE ( 'NONE', *, *, #2608, .T. ) ;
#3254 = DIRECTION ( 'NONE',  ( -0.000000000000000000, -0.000000000000000000, 1.000000000000000000 ) ) ;
#3255 = AXIS2_PLACEMENT_3D ( 'NONE', #5610, #2243, #4645 ) ;
#3256 = CARTESIAN_POINT ( 'NONE',  ( 9.192833548570416013, -59.02994620156847105, -35.00000000000000000 ) ) ;
#3257 = CONICAL_SURFACE ( 'NONE', #4448, 12.49999999999999822, 0.7853981633974501664 ) ;
#3258 = CARTESIAN_POINT ( 'NONE',  ( 27.60043906316099083, 27.60043906316109386, -35.00000000000000000 ) ) ;
#3259 = VECTOR ( 'NONE', #1797, 1000.000000000000000 ) ;
#3260 = AXIS2_PLACEMENT_3D ( 'NONE', #5642, #3274, #5179 ) ;
#3261 = CARTESIAN_POINT ( 'NONE',  ( -6.787591074359450971, -9.554964866038112348, 25.51646829178083919 ) ) ;
#3262 = VERTEX_POINT ( 'NONE', #144 ) ;
#3263 = CARTESIAN_POINT ( 'NONE',  ( 14.99999999999995559, -1.301042606982595854E-14, -35.00000000000000000 ) ) ;
#3264 = CIRCLE ( 'NONE', #4871, 5.000000000000004441 ) ;
#3265 = VERTEX_POINT ( 'NONE', #3580 ) ;
#3266 = EDGE_CURVE ( 'NONE', #2891, #3996, #2568, .T. ) ;
#3267 = DIRECTION ( 'NONE',  ( -1.154631945610162960E-14, 1.000000000000000000, 0.000000000000000000 ) ) ;
#3268 = ORIENTED_EDGE ( 'NONE', *, *, #1839, .T. ) ;
#3269 = CARTESIAN_POINT ( 'NONE',  ( 14.65251043020005461, -0.9663357036150953538, 38.18273246053423975 ) ) ;
#3270 = AXIS2_PLACEMENT_3D ( 'NONE', #3825, #4230, #557 ) ;
#3271 = CARTESIAN_POINT ( 'NONE',  ( 9.306281718482058096, -9.306281718482106058, 25.54332486258998358 ) ) ;
#3272 = ORIENTED_EDGE ( 'NONE', *, *, #1777, .F. ) ;
#3273 = ORIENTED_EDGE ( 'NONE', *, *, #1228, .T. ) ;
#3274 = DIRECTION ( 'NONE',  ( -0.000000000000000000, -0.000000000000000000, -1.000000000000000000 ) ) ;
#3275 = EDGE_CURVE ( 'NONE', #3523, #4211, #3264, .T. ) ;
#3276 = LINE ( 'NONE', #5180, #4717 ) ;
#3277 = CARTESIAN_POINT ( 'NONE',  ( -2.941541598353333735E-14, 7.604078429494112756E-14, -35.00000000000000000 ) ) ;
#3278 = DIRECTION ( 'NONE',  ( -0.000000000000000000, -0.000000000000000000, -1.000000000000000000 ) ) ;
#3279 = CARTESIAN_POINT ( 'NONE',  ( 13.90087379555094671, -4.954793796408218043, 38.30989703917857270 ) ) ;
#3280 = DIRECTION ( 'NONE',  ( 0.1538769332794359124, 0.9880900209011910240, 0.000000000000000000 ) ) ;
#3281 = ORIENTED_EDGE ( 'NONE', *, *, #1450, .T. ) ;
#3282 = EDGE_CURVE ( 'NONE', #1523, #2841, #3922, .T. ) ;
#3283 = CARTESIAN_POINT ( 'NONE',  ( -6.925838250501022308, 10.16165675636470489, 28.06531976343183743 ) ) ;
#3284 = ORIENTED_EDGE ( 'NONE', *, *, #3535, .T. ) ;
#3285 = CARTESIAN_POINT ( 'NONE',  ( -9.000000000000005329, 8.999999999988014920, 23.06137295785748265 ) ) ;
#3286 = VERTEX_POINT ( 'NONE', #5375 ) ;
#3287 = DIRECTION ( 'NONE',  ( 0.000000000000000000, 0.000000000000000000, 1.000000000000000000 ) ) ;
#3288 = CARTESIAN_POINT ( 'NONE',  ( -9.590870124851305079, -9.322893336083154736, 27.95908392747358207 ) ) ;
#3289 = DIRECTION ( 'NONE',  ( 1.000000000000000000, 0.000000000000000000, 0.000000000000000000 ) ) ;
#3290 = DIRECTION ( 'NONE',  ( -0.9880900209011910240, 0.1538769332794358846, 0.000000000000000000 ) ) ;
#3291 = ORIENTED_EDGE ( 'NONE', *, *, #2047, .T. ) ;
#3292 = DIRECTION ( 'NONE',  ( -0.9326495259660518844, 0.3607836771741465554, 0.000000000000000000 ) ) ;
#3293 = ORIENTED_EDGE ( 'NONE', *, *, #1408, .T. ) ;
#3294 = DIRECTION ( 'NONE',  ( 0.000000000000000000, 0.000000000000000000, 1.000000000000000000 ) ) ;
#3295 = DIRECTION ( 'NONE',  ( 0.000000000000000000, 1.000000000000000000, -0.000000000000000000 ) ) ;
#3296 = LINE ( 'NONE', #5272, #5228 ) ;
#3297 = VERTEX_POINT ( 'NONE', #3023 ) ;
#3298 = CARTESIAN_POINT ( 'NONE',  ( 0.000000000000000000, 0.000000000000000000, 205.0000000000000568 ) ) ;
#3299 = DIRECTION ( 'NONE',  ( 0.6273063437270283149, 0.7787725926866120307, -0.000000000000000000 ) ) ;
#3300 = VERTEX_POINT ( 'NONE', #1116 ) ;
#3301 = ORIENTED_EDGE ( 'NONE', *, *, #1494, .T. ) ;
#3302 = CARTESIAN_POINT ( 'NONE',  ( 12.00000000000000000, 0.000000000000000000, 35.00000000000000000 ) ) ;
#3303 = DIRECTION ( 'NONE',  ( -0.000000000000000000, -0.000000000000000000, 1.000000000000000000 ) ) ;
#3304 = CARTESIAN_POINT ( 'NONE',  ( 0.000000000000000000, 0.000000000000000000, 0.000000000000000000 ) ) ;
#3305 = CARTESIAN_POINT ( 'NONE',  ( 9.557272410707515320, 9.557272410707515320, 28.03893107092314096 ) ) ;
#3306 = CARTESIAN_POINT ( 'NONE',  ( 10.16167434176051820, -6.925743867604847281, 28.06532504456334109 ) ) ;
#3307 = ADVANCED_FACE ( 'NONE', ( #2997 ), #655, .F. ) ;
#3308 = ADVANCED_FACE ( 'NONE', ( #5875 ), #2196, .T. ) ;
#3309 = VERTEX_POINT ( 'NONE', #3636 ) ;
#3310 = CARTESIAN_POINT ( 'NONE',  ( 2.742560498089770427, 11.69030472852371005, 30.70728637550628548 ) ) ;
#3311 = CARTESIAN_POINT ( 'NONE',  ( 12.35760627049922533, 9.696021465980072307, 37.99999999999999289 ) ) ;
#3312 = CARTESIAN_POINT ( 'NONE',  ( 0.000000000000000000, 0.000000000000000000, 38.99999999999995737 ) ) ;
#3313 = ORIENTED_EDGE ( 'NONE', *, *, #4445, .F. ) ;
#3314 = CARTESIAN_POINT ( 'NONE',  ( -8.999999999988011368, -9.000000000000007105, 23.06137295785747909 ) ) ;
#3315 = ADVANCED_FACE ( 'NONE', ( #5497 ), #1278, .T. ) ;
#3316 = DIRECTION ( 'NONE',  ( 1.000000000000000000, 0.000000000000000000, -0.000000000000000000 ) ) ;
#3317 = LINE ( 'NONE', #379, #1829 ) ;
#3318 = CARTESIAN_POINT ( 'NONE',  ( 11.12736491637288516, 8.926329112024047774, 35.63514765224430647 ) ) ;
#3319 = CARTESIAN_POINT ( 'NONE',  ( -6.512188664276555627, -13.16119478149536270, 38.13833290264207676 ) ) ;
#3320 = ORIENTED_EDGE ( 'NONE', *, *, #4753, .F. ) ;
#3321 = DIRECTION ( 'NONE',  ( 1.000000000000000000, 0.000000000000000000, 0.000000000000000000 ) ) ;
#3322 = DIRECTION ( 'NONE',  ( 1.000000000000000000, 0.000000000000000000, 0.000000000000000000 ) ) ;
#3323 = DIRECTION ( 'NONE',  ( 0.000000000000000000, -0.000000000000000000, -1.000000000000000000 ) ) ;
#3324 = VERTEX_POINT ( 'NONE', #3115 ) ;
#3325 = DIRECTION ( 'NONE',  ( 1.000000000000000000, 0.000000000000000000, -0.000000000000000000 ) ) ;
#3326 = CARTESIAN_POINT ( 'NONE',  ( 3.878911688431552651, -13.33506331686138147, 35.78373290693656372 ) ) ;
#3327 = VECTOR ( 'NONE', #5945, 1000.000000000000000 ) ;
#3328 = ORIENTED_EDGE ( 'NONE', *, *, #2200, .T. ) ;
#3329 = EDGE_LOOP ( 'NONE', ( #3490, #3346, #2730, #5702, #183, #1685, #616, #3985, #3034, #2957, #2140, #1073, #4093, #1640, #3420, #4031 ) ) ;
#3330 = CARTESIAN_POINT ( 'NONE',  ( 9.192833548570215285, 59.02994620157096506, 35.00000000000000000 ) ) ;
#3331 = LINE ( 'NONE', #2405, #5825 ) ;
#3332 = CIRCLE ( 'NONE', #4117, 5.000000000000004441 ) ;
#3333 = CARTESIAN_POINT ( 'NONE',  ( 2.941541598353386116E-14, -7.604078429494091299E-14, -35.00000000000000000 ) ) ;
#3334 = CIRCLE ( 'NONE', #2343, 80.00000000000000000 ) ;
#3335 = FACE_OUTER_BOUND ( 'NONE', #3329, .T. ) ;
#3336 = VECTOR ( 'NONE', #4656, 999.9999999999998863 ) ;
#3337 = FACE_OUTER_BOUND ( 'NONE', #2431, .T. ) ;
#3338 = VERTEX_POINT ( 'NONE', #5880 ) ;
#3339 = ORIENTED_EDGE ( 'NONE', *, *, #2008, .F. ) ;
#3340 = CARTESIAN_POINT ( 'NONE',  ( 6.563799387313611788, 12.41448144607148230, 35.72511331161844339 ) ) ;
#3341 = CARTESIAN_POINT ( 'NONE',  ( 1.666666666666713814, 9.999999999999998224, 23.00000000000000000 ) ) ;
#3342 = DIRECTION ( 'NONE',  ( 1.000000000000000000, 0.000000000000000000, 0.000000000000000000 ) ) ;
#3343 = EDGE_CURVE ( 'NONE', #3966, #5881, #4762, .T. ) ;
#3344 = CIRCLE ( 'NONE', #1751, 12.49999999999999822 ) ;
#3345 = ADVANCED_FACE ( 'NONE', ( #4608 ), #3666, .F. ) ;
#3346 = ORIENTED_EDGE ( 'NONE', *, *, #4341, .T. ) ;
#3347 = CARTESIAN_POINT ( 'NONE',  ( -52.58482424179695158, -72.37680137756228760, -40.00000000000000000 ) ) ;
#3348 = CARTESIAN_POINT ( 'NONE',  ( -12.64046943599296924, -7.570233152424897582, 38.23931941266577894 ) ) ;
#3349 = CARTESIAN_POINT ( 'NONE',  ( -6.642184745761470666, -9.939337621248920840, 22.73823205004162773 ) ) ;
#3350 = EDGE_CURVE ( 'NONE', #3173, #1345, #4731, .T. ) ;
#3351 = DIRECTION ( 'NONE',  ( -1.000000000000000000, 0.000000000000000000, 0.000000000000000000 ) ) ;
#3352 = AXIS2_PLACEMENT_3D ( 'NONE', #1794, #5603, #4667 ) ;
#3353 = CARTESIAN_POINT ( 'NONE',  ( -8.952355667639968928, -11.66870637430388591, 38.09164563373219181 ) ) ;
#3354 = ORIENTED_EDGE ( 'NONE', *, *, #3529, .F. ) ;
#3355 = EDGE_CURVE ( 'NONE', #3286, #1252, #2974, .T. ) ;
#3356 = DIRECTION ( 'NONE',  ( -0.000000000000000000, -0.000000000000000000, -1.000000000000000000 ) ) ;
#3357 = AXIS2_PLACEMENT_3D ( 'NONE', #5492, #2229, #3689 ) ;
#3358 = DIRECTION ( 'NONE',  ( -0.000000000000000000, -0.000000000000000000, -1.000000000000000000 ) ) ;
#3359 = ORIENTED_EDGE ( 'NONE', *, *, #5799, .T. ) ;
#3360 = DIRECTION ( 'NONE',  ( 0.000000000000000000, 0.000000000000000000, 1.000000000000000000 ) ) ;
#3361 = VECTOR ( 'NONE', #2914, 1000.000000000000000 ) ;
#3362 = CARTESIAN_POINT ( 'NONE',  ( 9.157688896001733525, -8.975362584346067152, 22.85246612729343596 ) ) ;
#3363 = ORIENTED_EDGE ( 'NONE', *, *, #2520, .F. ) ;
#3364 = VERTEX_POINT ( 'NONE', #1426 ) ;
#3365 = CARTESIAN_POINT ( 'NONE',  ( 74.61196207728339402, 28.86269417393366865, 38.99999999999995737 ) ) ;
#3366 = DIRECTION ( 'NONE',  ( -0.3607836771741531612, -0.9326495259660494419, 0.000000000000000000 ) ) ;
#3367 = CARTESIAN_POINT ( 'NONE',  ( -12.00000000000000000, 0.000000000000000000, 20.00000000000000000 ) ) ;
#3368 = AXIS2_PLACEMENT_3D ( 'NONE', #2913, #63, #3351 ) ;
#3369 = CARTESIAN_POINT ( 'NONE',  ( -10.54244016040621190, -10.54244016040621013, 30.50000000000000000 ) ) ;
#3370 = CARTESIAN_POINT ( 'NONE',  ( 9.462636878983097688, -7.610208295502498999, 25.48187184588751464 ) ) ;
#3371 = ORIENTED_EDGE ( 'NONE', *, *, #2665, .T. ) ;
#3372 = CARTESIAN_POINT ( 'NONE',  ( 3.019346778933469810, 14.42236408824967775, 38.33740271606986738 ) ) ;
#3373 = CARTESIAN_POINT ( 'NONE',  ( -1.666666666666619223, 9.999999999999998224, 23.00000000000000000 ) ) ;
#3374 = DIRECTION ( 'NONE',  ( -0.000000000000000000, -0.000000000000000000, 1.000000000000000000 ) ) ;
#3375 = ORIENTED_EDGE ( 'NONE', *, *, #4636, .T. ) ;
#3376 = DIRECTION ( 'NONE',  ( 0.000000000000000000, 0.000000000000000000, 1.000000000000000000 ) ) ;
#3377 = CARTESIAN_POINT ( 'NONE',  ( -9.554965159330777169, -6.787634061845147393, 25.51646427192168431 ) ) ;
#3378 = CARTESIAN_POINT ( 'NONE',  ( -0.8289898103094419657, -9.900940235153617763, 22.73823205004162773 ) ) ;
#3379 = UNCERTAINTY_MEASURE_WITH_UNIT (LENGTH_MEASURE( 1.000000000000000082E-05 ), #6056, 'distance_accuracy_value', 'NONE');
#3380 = EDGE_CURVE ( 'NONE', #2060, #3100, #484, .T. ) ;
#3381 = CARTESIAN_POINT ( 'NONE',  ( 9.378998278013591872, 10.08321815271042610, 27.91486726096250948 ) ) ;
#3382 = CARTESIAN_POINT ( 'NONE',  ( 56.10121673609931037, 46.04269404270225863, 35.00000000000000000 ) ) ;
#3383 = EDGE_LOOP ( 'NONE', ( #5739, #295 ) ) ;
#3384 = LINE ( 'NONE', #5296, #62 ) ;
#3385 = CARTESIAN_POINT ( 'NONE',  ( 15.67638808697555142, 1.640158138686712206E-15, 38.00000000000000711 ) ) ;
#3386 = ORIENTED_EDGE ( 'NONE', *, *, #5948, .F. ) ;
#3387 = ADVANCED_FACE ( 'NONE', ( #4289 ), #2463, .T. ) ;
#3388 = FACE_BOUND ( 'NONE', #1271, .T. ) ;
#3389 = ADVANCED_FACE ( 'NONE', ( #1014, #5239 ), #4221, .T. ) ;
#3390 = CARTESIAN_POINT ( 'NONE',  ( 10.13908112636436520, -9.618700053625531154, 30.46372964425718521 ) ) ;
#3391 = ORIENTED_EDGE ( 'NONE', *, *, #5841, .T. ) ;
#3392 = SURFACE_SIDE_STYLE ('',( #4358 ) ) ;
#3393 = ORIENTED_EDGE ( 'NONE', *, *, #5560, .F. ) ;
#3394 = PLANE ( 'NONE',  #2167 ) ;
#3395 = LINE ( 'NONE', #987, #2637 ) ;
#3396 = CARTESIAN_POINT ( 'NONE',  ( 53.00449051625233210, 109.2944252875013262, 8.673617379884035472E-16 ) ) ;
#3397 = LINE ( 'NONE', #3369, #5373 ) ;
#3398 = CARTESIAN_POINT ( 'NONE',  ( 8.964415574088988592, -6.652784304366590185, 22.96342341013486887 ) ) ;
#3399 = ORIENTED_EDGE ( 'NONE', *, *, #2935, .F. ) ;
#3400 = CARTESIAN_POINT ( 'NONE',  ( 5.533593864557681208, 11.98089146579572883, 33.20390238845318009 ) ) ;
#3401 = FACE_OUTER_BOUND ( 'NONE', #3517, .T. ) ;
#3402 = CARTESIAN_POINT ( 'NONE',  ( 15.00000000000000000, 50.91502622129181788, 35.00000000000000000 ) ) ;
#3403 = EDGE_LOOP ( 'NONE', ( #290, #1507, #4130, #3893, #111 ) ) ;
#3404 = FACE_OUTER_BOUND ( 'NONE', #5955, .T. ) ;
#3405 = CARTESIAN_POINT ( 'NONE',  ( -9.793778397576030414, -8.539045536263005332, 27.99842134739335009 ) ) ;
#3406 = ORIENTED_EDGE ( 'NONE', *, *, #596, .T. ) ;
#3407 = EDGE_CURVE ( 'NONE', #3100, #4900, #1888, .T. ) ;
#3408 = CARTESIAN_POINT ( 'NONE',  ( 1.666666666666619223, -9.999999999999998224, 23.00000000000000000 ) ) ;
#3409 = LINE ( 'NONE', #935, #3748 ) ;
#3410 = CARTESIAN_POINT ( 'NONE',  ( 0.000000000000000000, 0.000000000000000000, 38.99999999999995737 ) ) ;
#3411 = VERTEX_POINT ( 'NONE', #5638 ) ;
#3412 = CARTESIAN_POINT ( 'NONE',  ( -10.00000000000000178, 10.00000000000000178, 20.00000000000000000 ) ) ;
#3413 = DIRECTION ( 'NONE',  ( 1.000000000000000000, 0.000000000000000000, 0.000000000000000000 ) ) ;
#3414 = EDGE_CURVE ( 'NONE', #816, #1974, #3783, .T. ) ;
#3415 = EDGE_CURVE ( 'NONE', #2529, #5460, #758, .T. ) ;
#3416 = CARTESIAN_POINT ( 'NONE',  ( 12.00215801354769063, 70.99259259259262933, 35.00000000000000000 ) ) ;
#3417 = EDGE_LOOP ( 'NONE', ( #78, #1738, #3769, #1957 ) ) ;
#3418 = CARTESIAN_POINT ( 'NONE',  ( -12.31015466235523981, 79.04720167209522685, 38.99999999999995737 ) ) ;
#3419 = CARTESIAN_POINT ( 'NONE',  ( 6.400384853991321066, -11.71459457793454995, 33.18278774224378225 ) ) ;
#3420 = ORIENTED_EDGE ( 'NONE', *, *, #2807, .T. ) ;
#3421 = SURFACE_STYLE_USAGE ( .BOTH. , #3392 ) ;
#3422 = CIRCLE ( 'NONE', #2635, 4.999999999999997335 ) ;
#3423 = ORIENTED_EDGE ( 'NONE', *, *, #5072, .T. ) ;
#3424 = CARTESIAN_POINT ( 'NONE',  ( 13.90645689909075777, 4.715863500831550148, 38.16097513848706768 ) ) ;
#3425 = DIRECTION ( 'NONE',  ( -0.7787725926866162496, 0.6273063437270229858, 0.000000000000000000 ) ) ;
#3426 = DIRECTION ( 'NONE',  ( -0.8922982081310915081, 0.4514464616829367838, 0.000000000000000000 ) ) ;
#3427 = EDGE_CURVE ( 'NONE', #3444, #429, #6060, .T. ) ;
#3428 = FACE_OUTER_BOUND ( 'NONE', #3581, .T. ) ;
#3429 = DIRECTION ( 'NONE',  ( 1.000000000000000000, 0.000000000000000000, 0.000000000000000000 ) ) ;
#3430 = ORIENTED_EDGE ( 'NONE', *, *, #4059, .T. ) ;
#3431 = AXIS2_PLACEMENT_3D ( 'NONE', #2621, #3577, #1305 ) ;
#3432 = B_SPLINE_CURVE_WITH_KNOTS ( 'NONE', 3,
 ( #4778, #3792, #5679, #3305, #2339, #5706 ),
 .UNSPECIFIED., .F., .F.,
 ( 4, 2, 4 ),
 ( 2.991083261082871196E-05, 0.007589224902417050257, 0.01514853897222326155 ),
 .UNSPECIFIED. ) ;
#3433 = EDGE_LOOP ( 'NONE', ( #851, #1824, #2358, #3737, #2676, #3757, #5003, #2283, #316, #5440 ) ) ;
#3434 = CARTESIAN_POINT ( 'NONE',  ( 5.247549479766072444, 10.46302782743270932, 28.11481907968152427 ) ) ;
#3435 = CARTESIAN_POINT ( 'NONE',  ( 9.981067540164714202, 9.981067540164714202, 22.73823205004162418 ) ) ;
#3437 = AXIS2_PLACEMENT_3D ( 'NONE', #3195, #2583, #967 ) ;
#3436 = DIRECTION ( 'NONE',  ( -0.000000000000000000, 0.000000000000000000, 1.000000000000000000 ) ) ;
#3438 = CIRCLE ( 'NONE', #4216, 80.00000000000002842 ) ;
#3439 = EDGE_CURVE ( 'NONE', #5370, #1998, #5760, .T. ) ;
#3440 = ORIENTED_EDGE ( 'NONE', *, *, #818, .F. ) ;
#3441 = LINE ( 'NONE', #2847, #1937 ) ;
#3442 = AXIS2_PLACEMENT_3D ( 'NONE', #2155, #1231, #2092 ) ;
#3443 = CARTESIAN_POINT ( 'NONE',  ( -11.79778917763282209, -1.839621235173125369, 30.71783072571432882 ) ) ;
#3444 = VERTEX_POINT ( 'NONE', #4318 ) ;
#3445 = DIRECTION ( 'NONE',  ( -1.000000000000000000, 0.000000000000000000, 0.000000000000000000 ) ) ;
#3446 = VECTOR ( 'NONE', #94, 1000.000000000000000 ) ;
#3447 = CARTESIAN_POINT ( 'NONE',  ( 11.58282027941459091, 3.645499761006323780, 30.69674202529824925 ) ) ;
#3448 = CARTESIAN_POINT ( 'NONE',  ( 5.114554293134526134E-14, 6.349488965209711204E-14, -35.00000000000000000 ) ) ;
#3449 = ORIENTED_EDGE ( 'NONE', *, *, #675, .T. ) ;
#3450 = CARTESIAN_POINT ( 'NONE',  ( 12.00000000000000000, 12.00000000000000355, -20.00000000000000000 ) ) ;
#3451 = SURFACE_SIDE_STYLE ('',( #673 ) ) ;
#3452 = DIRECTION ( 'NONE',  ( -0.000000000000000000, -0.000000000000000000, -1.000000000000000000 ) ) ;
#3453 = PRESENTATION_LAYER_ASSIGNMENT (  '', '', ( #3158 ) ) ;
#3454 = CARTESIAN_POINT ( 'NONE',  ( -2.830884587392779039, -12.60026679007841643, 33.25110354061416018 ) ) ;
#3455 = EDGE_CURVE ( 'NONE', #404, #1987, #72, .T. ) ;
#3456 = ORIENTED_EDGE ( 'NONE', *, *, #1972, .T. ) ;
#3457 = ORIENTED_EDGE ( 'NONE', *, *, #742, .T. ) ;
#3458 = LINE ( 'NONE', #3917, #992 ) ;
#3459 = CARTESIAN_POINT ( 'NONE',  ( 0.000000000000000000, 67.50000000000000000, 19.00000000000001066 ) ) ;
#3460 = AXIS2_PLACEMENT_3D ( 'NONE', #2954, #1516, #3413 ) ;
#3461 = DIRECTION ( 'NONE',  ( 0.000000000000000000, 0.000000000000000000, 1.000000000000000000 ) ) ;
#3462 = DIRECTION ( 'NONE',  ( -0.000000000000000000, -0.000000000000000000, -1.000000000000000000 ) ) ;
#3463 = CONICAL_SURFACE ( 'NONE', #4652, 80.00000000000000000, 0.7853981633974482790 ) ;
#3464 = AXIS2_PLACEMENT_3D ( 'NONE', #4876, #1195, #2081 ) ;
#3465 = ADVANCED_FACE ( 'NONE', ( #5770, #1492, #2329, #6135, #3388, #1858, #5301, #1043, #2919, #5456, #4924, #2989 ), #4985, .T. ) ;
#3466 = VERTEX_POINT ( 'NONE', #3418 ) ;
#3467 = CARTESIAN_POINT ( 'NONE',  ( 9.994658916190592990, 8.983694681928700021, 22.80938439471025703 ) ) ;
#3468 = CARTESIAN_POINT ( 'NONE',  ( 13.47611570251764412, -8.069545871843434526, 37.99999999999999289 ) ) ;
#3469 = CARTESIAN_POINT ( 'NONE',  ( -6.247143215332724651E-13, -89.46264649666795776, 40.00000000000000000 ) ) ;
#3470 = VERTEX_POINT ( 'NONE', #732 ) ;
#3471 = DIRECTION ( 'NONE',  ( 1.000000000000000000, 0.000000000000000000, 0.000000000000000000 ) ) ;
#3472 = CIRCLE ( 'NONE', #4769, 80.00000000000000000 ) ;
#3473 = EDGE_CURVE ( 'NONE', #4944, #1157, #1284, .T. ) ;
#3474 = CARTESIAN_POINT ( 'NONE',  ( -14.74111653287705792, -1.380323371794770872E-15, 38.35393095385146012 ) ) ;
#3475 = ORIENTED_EDGE ( 'NONE', *, *, #3951, .T. ) ;
#3476 = CARTESIAN_POINT ( 'NONE',  ( -7.178663235509287865, -13.97471987708211039, 38.00000000000000000 ) ) ;
#3477 = CARTESIAN_POINT ( 'NONE',  ( 10.77711034800893053, 7.077301327650772578, 30.61076202992614270 ) ) ;
#3478 = DIRECTION ( 'NONE',  ( -1.000000000000000000, 0.000000000000000000, 0.000000000000000000 ) ) ;
#3479 = ORIENTED_EDGE ( 'NONE', *, *, #3194, .F. ) ;
#3480 = DIRECTION ( 'NONE',  ( 0.000000000000000000, 0.000000000000000000, 1.000000000000000000 ) ) ;
#3481 = DIRECTION ( 'NONE',  ( 0.000000000000000000, -0.000000000000000000, 1.000000000000000000 ) ) ;
#3482 = CARTESIAN_POINT ( 'NONE',  ( 1.902479615894475451, -12.74240908541723982, 33.26151609189631841 ) ) ;
#3483 = EDGE_LOOP ( 'NONE', ( #1192, #597, #5167, #3138 ) ) ;
#3484 = CARTESIAN_POINT ( 'NONE',  ( 67.48246767247772482, 25.10212255632982092, 35.00000000000000000 ) ) ;
#3485 = ORIENTED_EDGE ( 'NONE', *, *, #4457, .T. ) ;
#3486 = DIRECTION ( 'NONE',  ( -0.5000000000000039968, 0.8660254037844363761, 0.000000000000000000 ) ) ;
#3487 = PLANE ( 'NONE',  #1187 ) ;
#3488 = CARTESIAN_POINT ( 'NONE',  ( 57.58482424179591419, -72.37680137756305498, 40.00000000000000000 ) ) ;
#3489 = CARTESIAN_POINT ( 'NONE',  ( -9.999999999999998224, -9.999999999999998224, 23.00000000000000000 ) ) ;
#3490 = ORIENTED_EDGE ( 'NONE', *, *, #4954, .F. ) ;
#3491 = CARTESIAN_POINT ( 'NONE',  ( 8.321939193476740826, 8.970286671637149212, 22.89273732682886475 ) ) ;
#3492 = CARTESIAN_POINT ( 'NONE',  ( 9.999999999999998224, -6.666666666666693608, 23.00000000000000000 ) ) ;
#3493 = EDGE_CURVE ( 'NONE', #2868, #5932, #1189, .T. ) ;
#3494 = EDGE_CURVE ( 'NONE', #2051, #3675, #4387, .T. ) ;
#3495 = ORIENTED_EDGE ( 'NONE', *, *, #3343, .T. ) ;
#3496 = DIRECTION ( 'NONE',  ( 0.9880900209011910240, -0.1538769332794358846, 0.000000000000000000 ) ) ;
#3497 = CARTESIAN_POINT ( 'NONE',  ( -11.85339260696609287, 0.9193131588476503024, 30.72304697887226510 ) ) ;
#3498 = ORIENTED_EDGE ( 'NONE', *, *, #1098, .T. ) ;
#3499 = FACE_BOUND ( 'NONE', #3767, .T. ) ;
#3500 = EDGE_CURVE ( 'NONE', #3324, #4272, #4898, .T. ) ;
#3501 = CARTESIAN_POINT ( 'NONE',  ( 8.963431230391419646, 4.154428044945160714, 23.04275563843252783 ) ) ;
#3502 = LINE ( 'NONE', #5306, #1823 ) ;
#3503 = ORIENTED_EDGE ( 'NONE', *, *, #1200, .F. ) ;
#3504 = LINE ( 'NONE', #706, #3723 ) ;
#3505 = DIRECTION ( 'NONE',  ( -0.000000000000000000, 0.000000000000000000, 1.000000000000000000 ) ) ;
#3506 = CARTESIAN_POINT ( 'NONE',  ( -2.035630462091350790, -14.63234267792704735, 38.34842398122203377 ) ) ;
#3507 = EDGE_LOOP ( 'NONE', ( #5769, #3230, #5311, #139 ) ) ;
#3508 = CARTESIAN_POINT ( 'NONE',  ( -5.141101056459331353, 67.50000000000000000, 28.99999999999999645 ) ) ;
#3509 = ORIENTED_EDGE ( 'NONE', *, *, #1519, .T. ) ;
#3510 = CARTESIAN_POINT ( 'NONE',  ( 11.94400843721214756, 8.542271628752923007, 38.10037361971538417 ) ) ;
#3511 = DIRECTION ( 'NONE',  ( -1.000000000000000000, 0.000000000000000000, 0.000000000000000000 ) ) ;
#3512 = APPLICATION_PROTOCOL_DEFINITION ( 'draft international standard', 'automotive_design', 1998, #487 ) ;
#3513 = CARTESIAN_POINT ( 'NONE',  ( 5.000000000000003553, 89.46264649666795776, -79.99999999999998579 ) ) ;
#3514 = FACE_OUTER_BOUND ( 'NONE', #4102, .T. ) ;
#3515 = PRODUCT_RELATED_PRODUCT_CATEGORY ( 'part', '', ( #4738 ) ) ;
#3516 = CIRCLE ( 'NONE', #5025, 2.499999999999998668 ) ;
#3517 = EDGE_LOOP ( 'NONE', ( #1555, #3293, #4891, #5714, #2485 ) ) ;
#3518 = DIRECTION ( 'NONE',  ( -1.000000000000000000, 0.000000000000000000, 0.000000000000000000 ) ) ;
#3519 = CARTESIAN_POINT ( 'NONE',  ( 9.930636381741159369, -5.809855716632679190, 22.73823205004162418 ) ) ;
#3520 = DIRECTION ( 'NONE',  ( 0.000000000000000000, 0.000000000000000000, 1.000000000000000000 ) ) ;
#3521 = VECTOR ( 'NONE', #5584, 1000.000000000000000 ) ;
#3522 = VECTOR ( 'NONE', #5768, 1000.000000000000000 ) ;
#3523 = VERTEX_POINT ( 'NONE', #166 ) ;
#3524 = CARTESIAN_POINT ( 'NONE',  ( 0.000000000000000000, 0.000000000000000000, -40.00000000000000000 ) ) ;
#3525 = CARTESIAN_POINT ( 'NONE',  ( -13.77854189090673742, 6.848566431882100464E-15, 35.81030296219172726 ) ) ;
#3526 =( REPRESENTATION_RELATIONSHIP ('NONE','NONE', #4716, #2176 ) REPRESENTATION_RELATIONSHIP_WITH_TRANSFORMATION ( #2295 )SHAPE_REPRESENTATION_RELATIONSHIP( ) );
#3527 = VERTEX_POINT ( 'NONE', #136 ) ;
#3528 = CARTESIAN_POINT ( 'NONE',  ( -9.086808451283777899, 11.58129469348872753, 38.17632780249462598 ) ) ;
#3529 = EDGE_CURVE ( 'NONE', #5996, #3051, #5967, .T. ) ;
#3530 = CARTESIAN_POINT ( 'NONE',  ( -80.00000000000000000, 9.797174393178826052E-15, 38.99999999999995737 ) ) ;
#3531 = CIRCLE ( 'NONE', #2547, 12.50000000000138733 ) ;
#3532 = VECTOR ( 'NONE', #5287, 1000.000000000000000 ) ;
#3533 = CIRCLE ( 'NONE', #2450, 5.000000000000004441 ) ;
#3534 = CARTESIAN_POINT ( 'NONE',  ( 10.16165675636470489, 6.925838250501023197, 28.06531976343183743 ) ) ;
#3535 = EDGE_CURVE ( 'NONE', #1135, #4471, #3472, .T. ) ;
#3536 = PRODUCT_DEFINITION_FORMATION_WITH_SPECIFIED_SOURCE ( 'ANY', '', #2845, .NOT_KNOWN. ) ;
#3537 = CARTESIAN_POINT ( 'NONE',  ( -85.08403291566612836, -27.64547812922793923, -40.00000000000000000 ) ) ;
#3538 = ORIENTED_EDGE ( 'NONE', *, *, #5378, .F. ) ;
#3539 = FACE_OUTER_BOUND ( 'NONE', #4610, .T. ) ;
#3540 = LINE ( 'NONE', #3911, #212 ) ;
#3541 = CARTESIAN_POINT ( 'NONE',  ( -1.776706711792240379, -10.85317354580219451, 28.17414650202874782 ) ) ;
#3542 = EDGE_CURVE ( 'NONE', #4405, #5737, #3540, .T. ) ;
#3543 = ORIENTED_EDGE ( 'NONE', *, *, #366, .F. ) ;
#3544 = CARTESIAN_POINT ( 'NONE',  ( 0.000000000000000000, 50.91502622129181788, 20.00000000000000000 ) ) ;
#3545 = ORIENTED_EDGE ( 'NONE', *, *, #2126, .F. ) ;
#3546 = FACE_OUTER_BOUND ( 'NONE', #1911, .T. ) ;
#3547 = FACE_OUTER_BOUND ( 'NONE', #349, .T. ) ;
#3548 = SHAPE_DEFINITION_REPRESENTATION ( #3191, #5596 ) ;
#3549 = LINE ( 'NONE', #1169, #4879 ) ;
#3550 = DIRECTION ( 'NONE',  ( 0.000000000000000000, -0.000000000000000000, -1.000000000000000000 ) ) ;
#3551 = ORIENTED_EDGE ( 'NONE', *, *, #1593, .F. ) ;
#3552 = VECTOR ( 'NONE', #4258, 1000.000000000000000 ) ;
#3553 = ORIENTED_EDGE ( 'NONE', *, *, #3189, .T. ) ;
#3554 = DIRECTION ( 'NONE',  ( 0.8660254037844385966, -0.5000000000000001110, 0.000000000000000000 ) ) ;
#3555 = CARTESIAN_POINT ( 'NONE',  ( 9.930636381741159369, 5.809855716632613465, 22.73823205004162418 ) ) ;
#3556 = DIRECTION ( 'NONE',  ( -0.000000000000000000, 0.000000000000000000, 1.000000000000000000 ) ) ;
#3557 = ORIENTED_EDGE ( 'NONE', *, *, #1371, .F. ) ;
#3558 = AXIS2_PLACEMENT_3D ( 'NONE', #2899, #4801, #1864 ) ;
#3559 = CARTESIAN_POINT ( 'NONE',  ( -11.69030472852370828, 2.742560498089769538, 30.70728637550628548 ) ) ;
#3560 = EDGE_LOOP ( 'NONE', ( #3970, #3391, #5664, #2786, #4475, #3814, #5198 ) ) ;
#3561 = FACE_BOUND ( 'NONE', #4799, .T. ) ;
#3562 = VECTOR ( 'NONE', #4510, 1000.000000000000000 ) ;
#3563 = VECTOR ( 'NONE', #1963, 1000.000000000000000 ) ;
#3564 = CARTESIAN_POINT ( 'NONE',  ( 9.554965159330777169, 6.787634061845148281, 25.51646427192168431 ) ) ;
#3565 = DIRECTION ( 'NONE',  ( -0.000000000000000000, -0.000000000000000000, 1.000000000000000000 ) ) ;
#3566 = VERTEX_POINT ( 'NONE', #5366 ) ;
#3567 = CARTESIAN_POINT ( 'NONE',  ( -9.144590365090015993, 9.969668718019493170, 22.73823205004162418 ) ) ;
#3568 = EDGE_CURVE ( 'NONE', #5932, #5813, #1215, .T. ) ;
#3569 = CARTESIAN_POINT ( 'NONE',  ( 2.035738251814313671, -14.63232105816060979, 38.34842656511671066 ) ) ;
#3570 = ORIENTED_EDGE ( 'NONE', *, *, #4538, .F. ) ;
#3571 = CARTESIAN_POINT ( 'NONE',  ( 68.32682326288126262, 26.05379589900813997, 35.04915833130704073 ) ) ;
#3572 = ORIENTED_EDGE ( 'NONE', *, *, #5455, .F. ) ;
#3573 = CARTESIAN_POINT ( 'NONE',  ( 12.00000000000000000, 50.91502622129181788, 35.00000000000000000 ) ) ;
#3574 = CARTESIAN_POINT ( 'NONE',  ( 7.182140071210238271E-14, -8.916303653273167033E-14, 35.00000000000000000 ) ) ;
#3575 = PRODUCT_CONTEXT ( 'NONE', #5891, 'mechanical' ) ;
#3576 = EDGE_CURVE ( 'NONE', #2489, #3996, #309, .T. ) ;
#3577 = DIRECTION ( 'NONE',  ( 0.5000000000000001110, 0.8660254037844385966, -0.000000000000000000 ) ) ;
#3578 = EDGE_CURVE ( 'NONE', #4471, #2132, #2838, .T. ) ;
#3579 = ADVANCED_BREP_SHAPE_REPRESENTATION ( '', ( #2153, #73 ), #1747 ) ;
#3580 = CARTESIAN_POINT ( 'NONE',  ( -80.08403291566614257, -27.64547812922793923, 40.00000000000000000 ) ) ;
#3581 = EDGE_LOOP ( 'NONE', ( #2867, #984, #1108, #4264 ) ) ;
#3582 = CARTESIAN_POINT ( 'NONE',  ( 9.515772848102855619, 10.27564057804868902, 33.05475024408053031 ) ) ;
#3583 = DIRECTION ( 'NONE',  ( -0.000000000000000000, 0.000000000000000000, 1.000000000000000000 ) ) ;
#3584 = DIRECTION ( 'NONE',  ( 0.000000000000000000, 0.000000000000000000, 1.000000000000000000 ) ) ;
#3585 = ORIENTED_EDGE ( 'NONE', *, *, #1398, .T. ) ;
#3586 = DIRECTION ( 'NONE',  ( -0.000000000000000000, -0.000000000000000000, -1.000000000000000000 ) ) ;
#3587 = CARTESIAN_POINT ( 'NONE',  ( -8.967351122863068014, 7.487361748921663285, 22.92808036848186504 ) ) ;
#3588 = ORIENTED_EDGE ( 'NONE', *, *, #641, .T. ) ;
#3589 = CARTESIAN_POINT ( 'NONE',  ( 4.130675435985391572E-14, 1.067806758184284836E-13, 35.00000000000000000 ) ) ;
#3590 = SURFACE_STYLE_USAGE ( .BOTH. , #3451 ) ;
#3591 = EDGE_CURVE ( 'NONE', #4214, #4020, #5569, .T. ) ;
#3592 = FACE_OUTER_BOUND ( 'NONE', #2659, .T. ) ;
#3593 = PLANE ( 'NONE',  #4824 ) ;
#3594 = EDGE_LOOP ( 'NONE', ( #2918, #3925, #306, #696 ) ) ;
#3595 = DIRECTION ( 'NONE',  ( 1.000000000000000000, 0.000000000000000000, 0.000000000000000000 ) ) ;
#3596 = VERTEX_POINT ( 'NONE', #1052 ) ;
#3597 = CARTESIAN_POINT ( 'NONE',  ( 0.000000000000000000, 0.000000000000000000, 205.0000000000000568 ) ) ;
#3598 = EDGE_LOOP ( 'NONE', ( #644, #1428, #5177, #394, #1856, #3117 ) ) ;
#3599 = CARTESIAN_POINT ( 'NONE',  ( -58.45671475544968843, 33.74999999999987210, 35.00000000000000000 ) ) ;
#3600 = EDGE_CURVE ( 'NONE', #193, #537, #4742, .T. ) ;
#3601 = DIRECTION ( 'NONE',  ( -0.000000000000000000, -1.000000000000000000, -0.000000000000000000 ) ) ;
#3602 = CONTEXT_DEPENDENT_SHAPE_REPRESENTATION ( #2254, #5887 ) ;
#3603 = DIRECTION ( 'NONE',  ( 0.6273063437270283149, 0.7787725926866119197, -0.000000000000000000 ) ) ;
#3604 = DIRECTION ( 'NONE',  ( 1.000000000000000000, 0.000000000000000000, 0.000000000000000000 ) ) ;
#3605 = ORIENTED_EDGE ( 'NONE', *, *, #3910, .F. ) ;
#3606 = CARTESIAN_POINT ( 'NONE',  ( -12.00215801354939948, 70.99259259259233090, 35.00000000000000000 ) ) ;
#3607 = EDGE_CURVE ( 'NONE', #882, #1611, #3432, .T. ) ;
#3608 = CARTESIAN_POINT ( 'NONE',  ( 0.000000000000000000, 67.50000000000000000, -20.00000000000000000 ) ) ;
#3609 = FACE_OUTER_BOUND ( 'NONE', #3071, .T. ) ;
#3610 = FACE_OUTER_BOUND ( 'NONE', #4983, .T. ) ;
#3611 = ORIENTED_EDGE ( 'NONE', *, *, #1399, .F. ) ;
#3612 = CARTESIAN_POINT ( 'NONE',  ( 14.42236408824967597, -3.019346778933470254, 38.33740271606987449 ) ) ;
#3613 = CARTESIAN_POINT ( 'NONE',  ( -9.554964866038103466, 6.787591074359464294, 25.51646829178083564 ) ) ;
#3614 = ORIENTED_EDGE ( 'NONE', *, *, #1663, .T. ) ;
#3615 = EDGE_CURVE ( 'NONE', #4405, #1185, #3171, .T. ) ;
#3616 = FACE_BOUND ( 'NONE', #1491, .T. ) ;
#3617 = DIRECTION ( 'NONE',  ( -1.000000000000000000, 0.000000000000000000, 0.000000000000000000 ) ) ;
#3618 = AXIS2_PLACEMENT_3D ( 'NONE', #4023, #4949, #4111 ) ;
#3619 = AXIS2_PLACEMENT_3D ( 'NONE', #4316, #6102, #2890 ) ;
#3620 = LINE ( 'NONE', #4532, #5236 ) ;
#3621 = CIRCLE ( 'NONE', #6027, 72.00000000000004263 ) ;
#3622 = FACE_OUTER_BOUND ( 'NONE', #4515, .T. ) ;
#3623 = CARTESIAN_POINT ( 'NONE',  ( -9.166666666666657193, 9.999999999999998224, 23.00000000000000000 ) ) ;
#3624 = AXIS2_PLACEMENT_3D ( 'NONE', #5685, #1290, #503 ) ;
#3625 = CIRCLE ( 'NONE', #165, 5.000000000000005329 ) ;
#3626 = CARTESIAN_POINT ( 'NONE',  ( -7.570044180282074819, -12.64059746256323002, 38.23931193745811186 ) ) ;
#3627 = CIRCLE ( 'NONE', #2138, 9.999999999999996447 ) ;
#3628 = ORIENTED_EDGE ( 'NONE', *, *, #1483, .F. ) ;
#3629 = LINE ( 'NONE', #5547, #707 ) ;
#3630 = ORIENTED_EDGE ( 'NONE', *, *, #4636, .F. ) ;
#3631 = CARTESIAN_POINT ( 'NONE',  ( -1.630640067418198669E-13, 67.50000000000002842, 35.00000000000000000 ) ) ;
#3632 = AXIS2_PLACEMENT_3D ( 'NONE', #1716, #378, #1319 ) ;
#3633 = FACE_OUTER_BOUND ( 'NONE', #726, .T. ) ;
#3634 = CONTEXT_DEPENDENT_SHAPE_REPRESENTATION ( #2385, #459 ) ;
#3635 = DIRECTION ( 'NONE',  ( -0.000000000000000000, -0.000000000000000000, -1.000000000000000000 ) ) ;
#3636 = CARTESIAN_POINT ( 'NONE',  ( -100.0000000000000000, 0.000000000000000000, 39.00000000000007105 ) ) ;
#3637 =( GEOMETRIC_REPRESENTATION_CONTEXT ( 3 ) GLOBAL_UNCERTAINTY_ASSIGNED_CONTEXT ( ( #4122 ) ) GLOBAL_UNIT_ASSIGNED_CONTEXT ( ( #2307, #5185, #5335 ) ) REPRESENTATION_CONTEXT ( 'NONE', 'WORKASPACE' ) );
#3638 = ADVANCED_FACE ( 'NONE', ( #1469 ), #2474, .F. ) ;
#3639 = CARTESIAN_POINT ( 'NONE',  ( -9.999999999999998224, -9.999999999999998224, 23.00000000000000000 ) ) ;
#3640 = ORIENTED_EDGE ( 'NONE', *, *, #1901, .F. ) ;
#3641 = DIRECTION ( 'NONE',  ( 0.000000000000000000, 0.000000000000000000, 1.000000000000000000 ) ) ;
#3642 = LINE ( 'NONE', #3183, #5719 ) ;
#3643 = SURFACE_STYLE_USAGE ( .BOTH. , #4587 ) ;
#3644 = CARTESIAN_POINT ( 'NONE',  ( 9.928243323025455425, 0.8581648076837078420, 25.63579099555274965 ) ) ;
#3645 = EDGE_CURVE ( 'NONE', #4944, #3749, #3397, .T. ) ;
#3646 = AXIS2_PLACEMENT_3D ( 'NONE', #1393, #1952, #5271 ) ;
#3647 = CARTESIAN_POINT ( 'NONE',  ( -11.57174281757876955, 8.159736356077658570, 35.66679457777021867 ) ) ;
#3648 = EDGE_LOOP ( 'NONE', ( #4069, #1163, #6007, #3273 ) ) ;
#3649 = CARTESIAN_POINT ( 'NONE',  ( -7.228764404800519294, 11.39256393965315439, 33.15620429642044797 ) ) ;
#3650 = CARTESIAN_POINT ( 'NONE',  ( 52.58482424179643289, 72.37680137756268550, 40.00000000000000000 ) ) ;
#3651 = AXIS2_PLACEMENT_3D ( 'NONE', #4293, #5207, #44 ) ;
#3652 = PLANE ( 'NONE',  #4434 ) ;
#3653 = EDGE_CURVE ( 'NONE', #1017, #688, #1024, .T. ) ;
#3654 = AXIS2_PLACEMENT_3D ( 'NONE', #439, #2319, #6039 ) ;
#3655 = CARTESIAN_POINT ( 'NONE',  ( -9.192833548570215285, -59.02994620157096506, 35.00000000000000000 ) ) ;
#3656 = DIRECTION ( 'NONE',  ( -0.1538769332794488742, 0.9880900209011889146, 0.000000000000000000 ) ) ;
#3657 = AXIS2_PLACEMENT_3D ( 'NONE', #268, #3058, #629 ) ;
#3658 = AXIS2_PLACEMENT_3D ( 'NONE', #4297, #496, #2409 ) ;
#3659 = DIRECTION ( 'NONE',  ( 1.000000000000000000, 0.000000000000000000, 0.000000000000000000 ) ) ;
#3660 = VERTEX_POINT ( 'NONE', #2902 ) ;
#3661 = CARTESIAN_POINT ( 'NONE',  ( 0.000000000000000000, 0.000000000000000000, 40.00000000000000000 ) ) ;
#3662 = ORIENTED_EDGE ( 'NONE', *, *, #2064, .T. ) ;
#3663 = CYLINDRICAL_SURFACE ( 'NONE', #1966, 12.50000000000000355 ) ;
#3664 = CARTESIAN_POINT ( 'NONE',  ( 46.52501622030442974, -37.47620048660870395, 35.00000000000000000 ) ) ;
#3665 = PLANE ( 'NONE',  #2036 ) ;
#3666 = PLANE ( 'NONE',  #1771 ) ;
#3667 = DIRECTION ( 'NONE',  ( -0.000000000000000000, 0.000000000000000000, 1.000000000000000000 ) ) ;
#3668 = EDGE_CURVE ( 'NONE', #1820, #1302, #6111, .T. ) ;
#3669 = EDGE_LOOP ( 'NONE', ( #4359, #1638, #5172, #1217 ) ) ;
#3670 = DIRECTION ( 'NONE',  ( -0.9326495259660518844, 0.3607836771741464998, 0.000000000000000000 ) ) ;
#3671 = DIRECTION ( 'NONE',  ( -0.4999999999999920619, -0.8660254037844432595, 0.000000000000000000 ) ) ;
#3672 = LINE ( 'NONE', #3277, #86 ) ;
#3673 = CARTESIAN_POINT ( 'NONE',  ( 10.70751178813581284, -3.531766105781286136, 28.15279191876807374 ) ) ;
#3674 = CARTESIAN_POINT ( 'NONE',  ( -11.39263409468386712, 7.228600378928585535, 33.15620577507544908 ) ) ;
#3675 = VERTEX_POINT ( 'NONE', #1830 ) ;
#3676 = CARTESIAN_POINT ( 'NONE',  ( -7.570233152424900247, 12.64046943599296924, 38.23931941266579315 ) ) ;
#3677 = CARTESIAN_POINT ( 'NONE',  ( -54.99999999999990052, -21.27605460800010206, -35.00000000000000000 ) ) ;
#3678 = ADVANCED_FACE ( 'NONE', ( #990 ), #1004, .F. ) ;
#3679 = EDGE_CURVE ( 'NONE', #2846, #3566, #3730, .T. ) ;
#3680 = DIRECTION ( 'NONE',  ( -0.000000000000000000, -0.000000000000000000, -1.000000000000000000 ) ) ;
#3681 = CARTESIAN_POINT ( 'NONE',  ( -99.00000000000005684, 0.000000000000000000, 40.00000000000000000 ) ) ;
#3682 = CARTESIAN_POINT ( 'NONE',  ( -13.92731518891510945, 4.729006349282765420, 38.16144984630088288 ) ) ;
#3683 = ADVANCED_FACE ( 'NONE', ( #5182 ), #3755, .F. ) ;
#3684 = UNCERTAINTY_MEASURE_WITH_UNIT (LENGTH_MEASURE( 1.000000000000000082E-05 ), #1802, 'distance_accuracy_value', 'NONE');
#3685 = CARTESIAN_POINT ( 'NONE',  ( -6.400535080091638740, -11.71455171164206810, 33.18278799730942552 ) ) ;
#3686 = ORIENTED_EDGE ( 'NONE', *, *, #2015, .T. ) ;
#3687 = FACE_OUTER_BOUND ( 'NONE', #5877, .T. ) ;
#3688 = ORIENTED_EDGE ( 'NONE', *, *, #1857, .F. ) ;
#3689 = DIRECTION ( 'NONE',  ( 1.000000000000000000, 0.000000000000000000, 0.000000000000000000 ) ) ;
#3690 = CYLINDRICAL_SURFACE ( 'NONE', #2163, 15.67638808697555142 ) ;
#3691 = ITEM_DEFINED_TRANSFORMATION ( 'NONE', 'NONE', #1449,  #73 ) ;
#3692 = DIRECTION ( 'NONE',  ( -0.000000000000000000, -0.000000000000000000, -1.000000000000000000 ) ) ;
#3693 = CARTESIAN_POINT ( 'NONE',  ( -9.999999999999998224, 8.333333333333346360, 23.00000000000000000 ) ) ;
#3694 = DIRECTION ( 'NONE',  ( 0.000000000000000000, 0.000000000000000000, 1.000000000000000000 ) ) ;
#3695 = ORIENTED_EDGE ( 'NONE', *, *, #675, .F. ) ;
#3696 = CARTESIAN_POINT ( 'NONE',  ( 15.00000000000000178, 52.91502622129183209, 35.00000000000000000 ) ) ;
#3697 = FACE_OUTER_BOUND ( 'NONE', #2765, .T. ) ;
#3698 = CARTESIAN_POINT ( 'NONE',  ( 7.765009959110445337, 12.46305503907310452, 38.11687012676380704 ) ) ;
#3699 = CARTESIAN_POINT ( 'NONE',  ( 12.24723121994938779, -4.666652649023727228, 33.22501677959694177 ) ) ;
#3700 = CARTESIAN_POINT ( 'NONE',  ( -57.35713647667095927, -46.20154318182582642, 35.13717928826310555 ) ) ;
#3701 = ORIENTED_EDGE ( 'NONE', *, *, #4522, .F. ) ;
#3702 = CARTESIAN_POINT ( 'NONE',  ( -5.533593864557652786, 11.98089146579573061, 33.20390238845318720 ) ) ;
#3703 = FACE_OUTER_BOUND ( 'NONE', #5011, .T. ) ;
#3704 = VERTEX_POINT ( 'NONE', #4703 ) ;
#3705 = DIRECTION ( 'NONE',  ( -0.5000000000000037748, 0.8660254037844365982, 0.000000000000000000 ) ) ;
#3706 = EDGE_CURVE ( 'NONE', #5747, #1644, #3862, .T. ) ;
#3707 = LINE ( 'NONE', #5978, #687 ) ;
#3708 = CARTESIAN_POINT ( 'NONE',  ( -13.16326790094652210, 6.508032323544350461, 38.13839276770976028 ) ) ;
#3709 = AXIS2_PLACEMENT_3D ( 'NONE', #4295, #1605, #4228 ) ;
#3710 = EDGE_CURVE ( 'NONE', #3704, #764, #1190, .T. ) ;
#3711 = CARTESIAN_POINT ( 'NONE',  ( -7.077172123266715964, -10.77715421822219710, 30.61076540981939687 ) ) ;
#3712 = ORIENTED_EDGE ( 'NONE', *, *, #5637, .F. ) ;
#3713 = LINE ( 'NONE', #3263, #1452 ) ;
#3714 = ORIENTED_EDGE ( 'NONE', *, *, #1494, .F. ) ;
#3715 = DIRECTION ( 'NONE',  ( 1.000000000000000000, 0.000000000000000000, 0.000000000000000000 ) ) ;
#3716 = DIRECTION ( 'NONE',  ( 0.000000000000000000, 0.000000000000000000, 1.000000000000000000 ) ) ;
#3717 = CARTESIAN_POINT ( 'NONE',  ( 80.00000000000000000, 0.000000000000000000, 38.99999999999995737 ) ) ;
#3718 = ORIENTED_EDGE ( 'NONE', *, *, #2168, .T. ) ;
#3719 = DIRECTION ( 'NONE',  ( 0.1538769332794359124, 0.9880900209011910240, 0.000000000000000000 ) ) ;
#3720 = CIRCLE ( 'NONE', #179, 80.00000000000000000 ) ;
#3721 = ADVANCED_FACE ( 'NONE', ( #3335 ), #5249, .F. ) ;
#3722 = CARTESIAN_POINT ( 'NONE',  ( 27.60043906316099083, 27.60043906316109386, -35.00000000000000000 ) ) ;
#3723 = VECTOR ( 'NONE', #4476, 1000.000000000000000 ) ;
#3724 = ORIENTED_EDGE ( 'NONE', *, *, #2168, .F. ) ;
#3725 = CARTESIAN_POINT ( 'NONE',  ( 55.71784976887228424, -21.55374571496028224, 35.00000000000000000 ) ) ;
#3726 = DIRECTION ( 'NONE',  ( 0.4999999999999980016, 0.8660254037844398178, 0.000000000000000000 ) ) ;
#3727 = CARTESIAN_POINT ( 'NONE',  ( 9.999999999999998224, -9.999999999999998224, -167.0000000000000284 ) ) ;
#3729 =( NAMED_UNIT ( * ) SI_UNIT ( $, .STERADIAN. ) SOLID_ANGLE_UNIT ( ) );
#3728 = PRODUCT_DEFINITION_FORMATION_WITH_SPECIFIED_SOURCE ( 'ANY', '', #825, .NOT_KNOWN. ) ;
#3730 = LINE ( 'NONE', #1374, #403 ) ;
#3731 = PRESENTATION_LAYER_ASSIGNMENT (  '', '', ( #1947 ) ) ;
#3732 = CARTESIAN_POINT ( 'NONE',  ( 11.98089146579572883, -5.533593864557682096, 33.20390238845318009 ) ) ;
#3733 = CARTESIAN_POINT ( 'NONE',  ( -8.983694681928700021, 9.994658916190592990, 22.80938439471025703 ) ) ;
#3734 = VERTEX_POINT ( 'NONE', #3983 ) ;
#3735 = EDGE_LOOP ( 'NONE', ( #4808, #4256, #3201, #2554 ) ) ;
#3736 = PLANE ( 'NONE',  #3624 ) ;
#3737 = ORIENTED_EDGE ( 'NONE', *, *, #4145, .F. ) ;
#3738 = CARTESIAN_POINT ( 'NONE',  ( 0.000000000000000000, 0.000000000000000000, -35.00000000000000000 ) ) ;
#3739 = AXIS2_PLACEMENT_3D ( 'NONE', #3918, #2620, #3053 ) ;
#3740 = CARTESIAN_POINT ( 'NONE',  ( -74.61196207728360719, -28.86269417393315351, -35.00000000000000711 ) ) ;
#3741 = VECTOR ( 'NONE', #4578, 1000.000000000000000 ) ;
#3742 = DIRECTION ( 'NONE',  ( 0.1538769332794487910, -0.9880900209011889146, 0.000000000000000000 ) ) ;
#3743 = AXIS2_PLACEMENT_3D ( 'NONE', #3661, #6008, #1722 ) ;
#3744 = CIRCLE ( 'NONE', #4755, 4.999999999999990230 ) ;
#3745 = CARTESIAN_POINT ( 'NONE',  ( 10.27564057804868725, 9.515772848102850290, 33.05475024408053741 ) ) ;
#3746 = ORIENTED_EDGE ( 'NONE', *, *, #2324, .F. ) ;
#3747 = DIRECTION ( 'NONE',  ( -0.000000000000000000, 0.000000000000000000, 1.000000000000000000 ) ) ;
#3748 = VECTOR ( 'NONE', #4788, 1000.000000000000000 ) ;
#3749 = VERTEX_POINT ( 'NONE', #5807 ) ;
#3750 = CARTESIAN_POINT ( 'NONE',  ( -85.08403291566554572, 27.64547812922971914, 40.00000000000000000 ) ) ;
#3751 = PLANE ( 'NONE',  #3646 ) ;
#3752 = EDGE_CURVE ( 'NONE', #2272, #5491, #5900, .T. ) ;
#3753 =( NAMED_UNIT ( * ) PLANE_ANGLE_UNIT ( ) SI_UNIT ( $, .RADIAN. ) );
#3754 = ORIENTED_EDGE ( 'NONE', *, *, #5560, .T. ) ;
#3755 = TOROIDAL_SURFACE ( 'NONE', #2, 72.00000000000004263, 10.00000000000000000 ) ;
#3756 = CARTESIAN_POINT ( 'NONE',  ( 0.000000000000000000, 0.000000000000000000, 20.00000000000000000 ) ) ;
#3757 = ORIENTED_EDGE ( 'NONE', *, *, #1603, .F. ) ;
#3758 = ORIENTED_EDGE ( 'NONE', *, *, #1603, .T. ) ;
#3759 = DIRECTION ( 'NONE',  ( 1.000000000000000000, 0.000000000000000000, 0.000000000000000000 ) ) ;
#3760 = CARTESIAN_POINT ( 'NONE',  ( -15.00000000000000000, 50.91502622129181788, 20.00000000000000000 ) ) ;
#3761 = EDGE_CURVE ( 'NONE', #1713, #2020, #4365, .T. ) ;
#3762 = CARTESIAN_POINT ( 'NONE',  ( 100.0000000000000000, 1.224646799147353217E-14, 40.00000000000000000 ) ) ;
#3763 = DIRECTION ( 'NONE',  ( 0.000000000000000000, 0.000000000000000000, 1.000000000000000000 ) ) ;
#3764 = ADVANCED_FACE ( 'NONE', ( #1996 ), #5374, .F. ) ;
#3765 = DIRECTION ( 'NONE',  ( -0.000000000000000000, 0.000000000000000000, 1.000000000000000000 ) ) ;
#3766 = DIRECTION ( 'NONE',  ( -1.000000000000000000, 0.000000000000000000, 0.000000000000000000 ) ) ;
#3767 = EDGE_LOOP ( 'NONE', ( #3879, #1876 ) ) ;
#3768 = CARTESIAN_POINT ( 'NONE',  ( -6.652779355836718977, 8.964415603276487232, 22.96342386064221941 ) ) ;
#3769 = ORIENTED_EDGE ( 'NONE', *, *, #3921, .F. ) ;
#3770 = DIRECTION ( 'NONE',  ( -0.1538769332794359124, -0.9880900209011910240, 0.000000000000000000 ) ) ;
#3771 = ORIENTED_EDGE ( 'NONE', *, *, #4538, .T. ) ;
#3772 = PLANE ( 'NONE',  #2236 ) ;
#3773 = CARTESIAN_POINT ( 'NONE',  ( -11.12736491637287983, -8.926329112024045997, 35.63514765224429226 ) ) ;
#3774 = CARTESIAN_POINT ( 'NONE',  ( -10.37777353962637505, 10.37777353962536608, 38.05103295300745003 ) ) ;
#3775 = PRODUCT_DEFINITION_SHAPE ( 'NONE', 'NONE',  #1387 ) ;
#3776 = CARTESIAN_POINT ( 'NONE',  ( 12.31015466235495026, 79.04720167209526949, 38.99999999999995737 ) ) ;
#3777 = CARTESIAN_POINT ( 'NONE',  ( 6.488003555186288906, -13.19914683770228336, 38.13881399654477633 ) ) ;
#3778 = ORIENTED_EDGE ( 'NONE', *, *, #2813, .F. ) ;
#3779 = DIRECTION ( 'NONE',  ( -0.000000000000000000, -0.000000000000000000, 1.000000000000000000 ) ) ;
#3780 = CARTESIAN_POINT ( 'NONE',  ( 9.192833548570416013, -59.02994620156847105, 35.00000000000000000 ) ) ;
#3781 = FACE_OUTER_BOUND ( 'NONE', #1095, .T. ) ;
#3782 = ORIENTED_EDGE ( 'NONE', *, *, #2087, .F. ) ;
#3783 = LINE ( 'NONE', #5203, #2581 ) ;
#3784 = CARTESIAN_POINT ( 'NONE',  ( 4.399300199984971016, -10.59948853791303769, 28.13666499103235452 ) ) ;
#3785 = ADVANCED_FACE ( 'NONE', ( #3428 ), #1087, .T. ) ;
#3786 = EDGE_CURVE ( 'NONE', #6095, #4944, #901, .T. ) ;
#3787 = EDGE_LOOP ( 'NONE', ( #4452, #171, #477, #567 ) ) ;
#3788 = VERTEX_POINT ( 'NONE', #1615 ) ;
#3789 = CARTESIAN_POINT ( 'NONE',  ( 81.00000000000004263, 0.000000000000000000, 40.00000000000000000 ) ) ;
#3790 = DIRECTION ( 'NONE',  ( 0.000000000000000000, 0.000000000000000000, -1.000000000000000000 ) ) ;
#3791 = DIRECTION ( 'NONE',  ( -0.9326495259660445569, -0.3607836771741652071, 0.000000000000000000 ) ) ;
#3792 = CARTESIAN_POINT ( 'NONE',  ( 10.19629538396769952, 10.19629538384312184, 35.54424335298406135 ) ) ;
#3793 = CARTESIAN_POINT ( 'NONE',  ( 12.01622299351614132, -7.392961014695930366, 35.69843844696170976 ) ) ;
#3794 = EDGE_CURVE ( 'NONE', #251, #4467, #5216, .T. ) ;
#3795 = EDGE_CURVE ( 'NONE', #1157, #936, #615, .T. ) ;
#3796 = ORIENTED_EDGE ( 'NONE', *, *, #1680, .F. ) ;
#3797 = CARTESIAN_POINT ( 'NONE',  ( 4.154433491267528034, 8.963431154120575783, 23.04275521548131067 ) ) ;
#3798 = CARTESIAN_POINT ( 'NONE',  ( -2.164213882025733060, 15.56315586465741951, 38.00000000000000711 ) ) ;
#3799 = CARTESIAN_POINT ( 'NONE',  ( -13.90645689909058369, -4.715863500832077726, 38.16097513848706058 ) ) ;
#3800 = VERTEX_POINT ( 'NONE', #740 ) ;
#3801 = CARTESIAN_POINT ( 'NONE',  ( -58.45671475544962448, -33.75000000000001421, 35.00000000000000000 ) ) ;
#3802 = ADVANCED_FACE ( 'NONE', ( #5401 ), #1141, .F. ) ;
#3803 = CARTESIAN_POINT ( 'NONE',  ( -10.50531938289192446, -7.869812776064875948, 30.57803900350706172 ) ) ;
#3804 = DIRECTION ( 'NONE',  ( -0.000000000000000000, -0.000000000000000000, -1.000000000000000000 ) ) ;
#3805 = UNCERTAINTY_MEASURE_WITH_UNIT (LENGTH_MEASURE( 1.000000000000000082E-05 ), #5845, 'distance_accuracy_value', 'NONE');
#3806 = CARTESIAN_POINT ( 'NONE',  ( 9.999999999999998224, -9.999999999999998224, 23.00000000000000000 ) ) ;
#3807 = CARTESIAN_POINT ( 'NONE',  ( 1.900794651634724719, -14.58443831393950418, 38.18056006088391996 ) ) ;
#3808 = EDGE_LOOP ( 'NONE', ( #1509, #5655, #546, #5484 ) ) ;
#3809 = CARTESIAN_POINT ( 'NONE',  ( 47.58482424179590708, -72.37680137756305498, -79.99999999999998579 ) ) ;
#3810 = CARTESIAN_POINT ( 'NONE',  ( 0.000000000000000000, 0.000000000000000000, 40.00000000000000000 ) ) ;
#3811 = AXIS2_PLACEMENT_3D ( 'NONE', #4701, #1370, #3671 ) ;
#3812 = AXIS2_PLACEMENT_3D ( 'NONE', #1953, #914, #1914 ) ;
#3813 = CARTESIAN_POINT ( 'NONE',  ( 0.000000000000000000, 67.50000000000000000, 35.00000000000000000 ) ) ;
#3814 = ORIENTED_EDGE ( 'NONE', *, *, #2448, .T. ) ;
#3815 = CARTESIAN_POINT ( 'NONE',  ( -85.08403291566554572, 27.64547812922971914, -40.00000000000000000 ) ) ;
#3816 = CARTESIAN_POINT ( 'NONE',  ( 10.38144361273100280, -10.38144361273100813, 38.10175261887127363 ) ) ;
#3817 = CIRCLE ( 'NONE', #2133, 2.499999999999998668 ) ;
#3818 = CIRCLE ( 'NONE', #1734, 12.50000000000138733 ) ;
#3819 = ORIENTED_EDGE ( 'NONE', *, *, #5982, .T. ) ;
#3820 = ORIENTED_EDGE ( 'NONE', *, *, #285, .T. ) ;
#3821 = PLANE ( 'NONE',  #1472 ) ;
#3822 = CARTESIAN_POINT ( 'NONE',  ( 0.000000000000000000, 0.000000000000000000, 38.99999999999995737 ) ) ;
#3823 = DIRECTION ( 'NONE',  ( 0.000000000000000000, 1.387778780781445676E-17, 1.000000000000000000 ) ) ;
#3824 = CIRCLE ( 'NONE', #471, 5.000000000000004441 ) ;
#3825 = CARTESIAN_POINT ( 'NONE',  ( 0.000000000000000000, 0.000000000000000000, 45.00000000000000711 ) ) ;
#3826 = AXIS2_PLACEMENT_3D ( 'NONE', #1414, #1537, #5223 ) ;
#3827 = CARTESIAN_POINT ( 'NONE',  ( 9.554964866038103466, -6.787591074359449195, 25.51646829178083564 ) ) ;
#3828 = CIRCLE ( 'NONE', #4629, 5.000000000000004441 ) ;
#3829 = AXIS2_PLACEMENT_3D ( 'NONE', #2472, #2435, #627 ) ;
#3830 = ORIENTED_EDGE ( 'NONE', *, *, #2636, .F. ) ;
#3831 = CARTESIAN_POINT ( 'NONE',  ( -0.8880320553140206297, 10.89081796499577415, 28.17941898721253580 ) ) ;
#3832 = CARTESIAN_POINT ( 'NONE',  ( 67.48246767247772482, 25.10212255632982092, 35.00000000000000000 ) ) ;
#3833 = CARTESIAN_POINT ( 'NONE',  ( 0.000000000000000000, 0.000000000000000000, -39.00000000000002842 ) ) ;
#3834 = AXIS2_PLACEMENT_3D ( 'NONE', #5894, #4005, #3948 ) ;
#3835 = EDGE_CURVE ( 'NONE', #4044, #3444, #213, .T. ) ;
#3836 = VERTEX_POINT ( 'NONE', #3891 ) ;
#3837 = CARTESIAN_POINT ( 'NONE',  ( 0.000000000000000000, 0.000000000000000000, -35.00000000000000000 ) ) ;
#3838 = CARTESIAN_POINT ( 'NONE',  ( -10.16165675636470134, -6.925838250501020532, 28.06531976343184098 ) ) ;
#3839 = CARTESIAN_POINT ( 'NONE',  ( 8.069545871843425644, -13.47611570251764412, 37.99999999999999289 ) ) ;
#3840 = AXIS2_PLACEMENT_3D ( 'NONE', #1372, #1801, #1340 ) ;
#3841 = EDGE_CURVE ( 'NONE', #5491, #537, #3549, .T. ) ;
#3842 = DIRECTION ( 'NONE',  ( -0.000000000000000000, 0.000000000000000000, 1.000000000000000000 ) ) ;
#3843 = AXIS2_PLACEMENT_3D ( 'NONE', #4097, #5109, #6013 ) ;
#3844 = CARTESIAN_POINT ( 'NONE',  ( -12.49999999999999822, -67.50000000000000000, 35.00000000000000000 ) ) ;
#3845 = EDGE_LOOP ( 'NONE', ( #2896, #5965, #5999, #2633 ) ) ;
#3846 = LINE ( 'NONE', #5796, #4346 ) ;
#3847 = VECTOR ( 'NONE', #1071, 1000.000000000000000 ) ;
#3848 = CIRCLE ( 'NONE', #1269, 12.50000000000138911 ) ;
#3849 = FACE_OUTER_BOUND ( 'NONE', #185, .T. ) ;
#3850 = ORIENTED_EDGE ( 'NONE', *, *, #1333, .T. ) ;
#3851 = CARTESIAN_POINT ( 'NONE',  ( 4.130675435985391572E-14, 1.067806758184284836E-13, 35.00000000000000000 ) ) ;
#3852 = VECTOR ( 'NONE', #2455, 1000.000000000000114 ) ;
#3853 = CARTESIAN_POINT ( 'NONE',  ( 8.662324224478984647, -10.23352841777491840, 30.54531597708798429 ) ) ;
#3854 = ORIENTED_EDGE ( 'NONE', *, *, #3236, .T. ) ;
#3855 = PRESENTATION_STYLE_ASSIGNMENT (( #3421 ) ) ;
#3856 = VERTEX_POINT ( 'NONE', #4425 ) ;
#3857 = AXIS2_PLACEMENT_3D ( 'NONE', #738, #177, #1589 ) ;
#3858 = CARTESIAN_POINT ( 'NONE',  ( -9.999999999999998224, -8.999999999999998224, 23.00000000000000000 ) ) ;
#3859 = LINE ( 'NONE', #2433, #3131 ) ;
#3860 = CARTESIAN_POINT ( 'NONE',  ( -10.37777353962477278, -10.37777353962696303, 38.05103295300743582 ) ) ;
#3861 = DIRECTION ( 'NONE',  ( -2.775557561562891351E-17, 0.000000000000000000, 1.000000000000000000 ) ) ;
#3862 = CIRCLE ( 'NONE', #4262, 9.500000000000005329 ) ;
#3863 = DIRECTION ( 'NONE',  ( 1.000000000000000000, 0.000000000000000000, 0.000000000000000000 ) ) ;
#3864 = CARTESIAN_POINT ( 'NONE',  ( 11.03292118881348394, -8.007183658747754507, 33.12420745160152791 ) ) ;
#3865 = VERTEX_POINT ( 'NONE', #3488 ) ;
#3866 = CARTESIAN_POINT ( 'NONE',  ( 2.654236408786762702, 10.78034266696900367, 28.16346921039841078 ) ) ;
#3867 = DIRECTION ( 'NONE',  ( 0.000000000000000000, 0.000000000000000000, 1.000000000000000000 ) ) ;
#3868 = CARTESIAN_POINT ( 'NONE',  ( -56.10121673609931037, -46.04269404270225863, 35.00000000000000000 ) ) ;
#3869 = ORIENTED_EDGE ( 'NONE', *, *, #2697, .T. ) ;
#3870 = DIRECTION ( 'NONE',  ( -0.8660254037844385966, 0.5000000000000001110, 0.000000000000000000 ) ) ;
#3871 = LINE ( 'NONE', #1844, #4743 ) ;
#3872 = ORIENTED_EDGE ( 'NONE', *, *, #2318, .F. ) ;
#3873 = EDGE_CURVE ( 'NONE', #559, #5737, #5426, .T. ) ;
#3874 = EDGE_CURVE ( 'NONE', #2223, #719, #3022, .T. ) ;
#3875 = CARTESIAN_POINT ( 'NONE',  ( 67.48246767247886169, -25.10212255632678691, 35.00000000000000000 ) ) ;
#3876 = CARTESIAN_POINT ( 'NONE',  ( 11.33314185116896589, 72.77350886803867525, 35.00000000000000000 ) ) ;
#3877 = ADVANCED_FACE ( 'NONE', ( #685 ), #1929, .F. ) ;
#3878 = CARTESIAN_POINT ( 'NONE',  ( 57.35713647667095927, 46.20154318182582642, 35.13717928826310555 ) ) ;
#3879 = ORIENTED_EDGE ( 'NONE', *, *, #4598, .T. ) ;
#3880 = DIRECTION ( 'NONE',  ( -0.000000000000000000, -0.000000000000000000, 1.000000000000000000 ) ) ;
#3881 = CARTESIAN_POINT ( 'NONE',  ( 54.99999999999999289, 6.349087922075113966E-13, 35.00000000000000000 ) ) ;
#3882 = CARTESIAN_POINT ( 'NONE',  ( 9.000000000000005329, -8.999999999988066435, 23.06137295785747554 ) ) ;
#3883 = ORIENTED_EDGE ( 'NONE', *, *, #1663, .F. ) ;
#3884 = CARTESIAN_POINT ( 'NONE',  ( 8.321944142006520551, -8.970286642449650572, 22.89273687632151422 ) ) ;
#3885 = EDGE_CURVE ( 'NONE', #6127, #2468, #2566, .T. ) ;
#3886 = VERTEX_POINT ( 'NONE', #4965 ) ;
#3887 = ORIENTED_EDGE ( 'NONE', *, *, #5176, .F. ) ;
#3888 = DIRECTION ( 'NONE',  ( 0.000000000000000000, 0.000000000000000000, 1.000000000000000000 ) ) ;
#3889 = DIRECTION ( 'NONE',  ( -0.000000000000000000, -0.000000000000000000, -1.000000000000000000 ) ) ;
#3890 = DIRECTION ( 'NONE',  ( 1.000000000000000000, 0.000000000000000000, 0.000000000000000000 ) ) ;
#3891 = CARTESIAN_POINT ( 'NONE',  ( -57.35713647667095927, -46.20154318182582642, -35.00000000000000000 ) ) ;
#3892 = CARTESIAN_POINT ( 'NONE',  ( 11.58116666691846319, -9.086997423426607767, 38.17633527770230017 ) ) ;
#3893 = ORIENTED_EDGE ( 'NONE', *, *, #4270, .T. ) ;
#3894 = ORIENTED_EDGE ( 'NONE', *, *, #5266, .T. ) ;
#3895 = CARTESIAN_POINT ( 'NONE',  ( 5.845970755595366164, 13.50805179034378867, 38.28811402100272687 ) ) ;
#3896 = CARTESIAN_POINT ( 'NONE',  ( 9.999999999999998224, 9.166666666666657193, 23.00000000000000000 ) ) ;
#3897 = CARTESIAN_POINT ( 'NONE',  ( 0.000000000000000000, 0.000000000000000000, 35.00000000000000000 ) ) ;
#3898 = ORIENTED_EDGE ( 'NONE', *, *, #5521, .F. ) ;
#3899 = FACE_OUTER_BOUND ( 'NONE', #3125, .T. ) ;
#3900 = CARTESIAN_POINT ( 'NONE',  ( -13.07368784376654780, -4.807938790076510926, 35.76776929191790089 ) ) ;
#3901 = ORIENTED_EDGE ( 'NONE', *, *, #41, .F. ) ;
#3902 = CARTESIAN_POINT ( 'NONE',  ( 4.166666666666626107, -9.999999999999998224, 23.00000000000000000 ) ) ;
#3903 = EDGE_CURVE ( 'NONE', #4711, #5893, #162, .T. ) ;
#3904 = CARTESIAN_POINT ( 'NONE',  ( 13.33506331686138147, 3.878911688431560201, 35.78373290693656372 ) ) ;
#3905 = CARTESIAN_POINT ( 'NONE',  ( 8.999999999999998224, -8.999999999999998224, 23.00000000000000000 ) ) ;
#3906 = VERTEX_POINT ( 'NONE', #1769 ) ;
#3907 = CARTESIAN_POINT ( 'NONE',  ( 85.08403291566592941, 27.64547812922851833, 40.00000000000000000 ) ) ;
#3908 = CARTESIAN_POINT ( 'NONE',  ( 1.131281550719567528E-13, 1.761763928569687004E-14, 35.00000000000000000 ) ) ;
#3909 = DIRECTION ( 'NONE',  ( 0.000000000000000000, 0.000000000000000000, 1.000000000000000000 ) ) ;
#3910 = EDGE_CURVE ( 'NONE', #719, #2891, #463, .T. ) ;
#3911 = CARTESIAN_POINT ( 'NONE',  ( 68.69027832783777399, 26.57196568621521138, 35.00000000000000000 ) ) ;
#3912 = CARTESIAN_POINT ( 'NONE',  ( 9.086808451283770793, -11.58129469348872220, 38.17632780249461888 ) ) ;
#3913 = ORIENTED_EDGE ( 'NONE', *, *, #3003, .F. ) ;
#3914 = CARTESIAN_POINT ( 'NONE',  ( -9.378998278013591872, 10.08321815271041721, 27.91486726096250948 ) ) ;
#3915 = VECTOR ( 'NONE', #2714, 1000.000000000000000 ) ;
#3916 = ORIENTED_EDGE ( 'NONE', *, *, #5377, .T. ) ;
#3917 = CARTESIAN_POINT ( 'NONE',  ( -14.99999999999995559, -1.301042606982600272E-14, -20.00000000000000000 ) ) ;
#3918 = CARTESIAN_POINT ( 'NONE',  ( 0.000000000000000000, 0.000000000000000000, 35.00000000000000000 ) ) ;
#3919 = CARTESIAN_POINT ( 'NONE',  ( 0.000000000000000000, 0.000000000000000000, 0.000000000000000000 ) ) ;
#3920 = DIRECTION ( 'NONE',  ( -0.000000000000000000, -0.000000000000000000, -1.000000000000000000 ) ) ;
#3921 = EDGE_CURVE ( 'NONE', #747, #5424, #332, .T. ) ;
#3922 = LINE ( 'NONE', #5844, #2172 ) ;
#3923 = VECTOR ( 'NONE', #823, 999.9999999999998863 ) ;
#3924 = VECTOR ( 'NONE', #6133, 1000.000000000000114 ) ;
#3925 = ORIENTED_EDGE ( 'NONE', *, *, #5261, .T. ) ;
#3926 = CARTESIAN_POINT ( 'NONE',  ( 2.830884587392778595, 12.60026679007841643, 33.25110354061416018 ) ) ;
#3927 = DIRECTION ( 'NONE',  ( 0.9326495259660518844, -0.3607836771741464998, 0.000000000000000000 ) ) ;
#3929 = CIRCLE ( 'NONE', #5722, 10.00000000000000178 ) ;
#3928 = CARTESIAN_POINT ( 'NONE',  ( -12.74784844745956747, -7.336363311097503725, 38.12594328983445280 ) ) ;
#3930 = AXIS2_PLACEMENT_3D ( 'NONE', #2667, #5393, #2956 ) ;
#3931 = EDGE_LOOP ( 'NONE', ( #1112, #3628, #3108, #5556, #5232 ) ) ;
#3932 = DIRECTION ( 'NONE',  ( 1.000000000000000000, 0.000000000000000000, 0.000000000000000000 ) ) ;
#3933 = AXIS2_PLACEMENT_3D ( 'NONE', #4850, #1029, #601 ) ;
#3934 = CARTESIAN_POINT ( 'NONE',  ( -9.908812100099982700, -1.716690548177160824, 25.63028262842344773 ) ) ;
#3935 = ORIENTED_EDGE ( 'NONE', *, *, #4999, .F. ) ;
#3936 = VECTOR ( 'NONE', #3880, 1000.000000000000000 ) ;
#3937 = CARTESIAN_POINT ( 'NONE',  ( -5.273949241992683667, -14.79903580929011930, 38.00000000000000711 ) ) ;
#3938 = AXIS2_PLACEMENT_3D ( 'NONE', #4327, #3861, #2929 ) ;
#3939 = CIRCLE ( 'NONE', #189, 12.50000000000138911 ) ;
#3940 = CARTESIAN_POINT ( 'NONE',  ( 10.59948853791303769, 4.399300199984972792, 28.13666499103235452 ) ) ;
#3941 = CARTESIAN_POINT ( 'NONE',  ( 99.00000000000005684, 1.212400331155880333E-14, 40.00000000000000000 ) ) ;
#3942 = ORIENTED_EDGE ( 'NONE', *, *, #5828, .F. ) ;
#3943 = CARTESIAN_POINT ( 'NONE',  ( -85.08403291566612836, -27.64547812922793923, 40.00000000000000000 ) ) ;
#3944 = CARTESIAN_POINT ( 'NONE',  ( 12.00000000000000000, 50.91502622129181788, -20.00000000000000000 ) ) ;
#3945 = VECTOR ( 'NONE', #35, 1000.000000000000000 ) ;
#3946 = CARTESIAN_POINT ( 'NONE',  ( -5.842721101324136525E-14, -9.928243323025430556, 25.63579099555279583 ) ) ;
#3947 = EDGE_LOOP ( 'NONE', ( #5674, #1905, #1455, #1281 ) ) ;
#3948 = DIRECTION ( 'NONE',  ( 1.000000000000000000, 0.000000000000000000, 0.000000000000000000 ) ) ;
#3949 = ORIENTED_EDGE ( 'NONE', *, *, #3473, .F. ) ;
#3950 = DIRECTION ( 'NONE',  ( 0.4999999999999980016, 0.8660254037844398178, 0.000000000000000000 ) ) ;
#3951 = EDGE_CURVE ( 'NONE', #5786, #945, #4134, .T. ) ;
#3952 = ADVANCED_FACE ( 'NONE', ( #267 ), #358, .F. ) ;
#3953 = CARTESIAN_POINT ( 'NONE',  ( -5.000000000000003553, 89.46264649666795776, 40.00000000000000000 ) ) ;
#3954 = AXIS2_PLACEMENT_3D ( 'NONE', #2206, #978, #1886 ) ;
#3955 = DIRECTION ( 'NONE',  ( 0.000000000000000000, 0.000000000000000000, 1.000000000000000000 ) ) ;
#3956 = DIRECTION ( 'NONE',  ( 0.000000000000000000, 0.000000000000000000, 1.000000000000000000 ) ) ;
#3957 = VECTOR ( 'NONE', #576, 1000.000000000000000 ) ;
#3958 = ORIENTED_EDGE ( 'NONE', *, *, #241, .T. ) ;
#3959 = VECTOR ( 'NONE', #920, 1000.000000000000000 ) ;
#3960 = ORIENTED_EDGE ( 'NONE', *, *, #531, .F. ) ;
#3961 = ADVANCED_FACE ( 'NONE', ( #1331 ), #3665, .F. ) ;
#3962 = CARTESIAN_POINT ( 'NONE',  ( 0.000000000000000000, 50.91502622129181788, 20.00000000000000000 ) ) ;
#3963 = AXIS2_PLACEMENT_3D ( 'NONE', #2535, #4426, #2059 ) ;
#3964 = LINE ( 'NONE', #5879, #4444 ) ;
#3965 = CARTESIAN_POINT ( 'NONE',  ( 11.33314185117008677, -72.77350886804093477, 35.13717928826310555 ) ) ;
#3966 = VERTEX_POINT ( 'NONE', #5579 ) ;
#3967 = VECTOR ( 'NONE', #447, 1000.000000000000114 ) ;
#3968 = CARTESIAN_POINT ( 'NONE',  ( -11.69030472852370295, -2.742560498089724241, 30.70728637550628193 ) ) ;
#3969 =( REPRESENTATION_RELATIONSHIP ('NONE','NONE', #4716, #5596 ) REPRESENTATION_RELATIONSHIP_WITH_TRANSFORMATION ( #3113 )SHAPE_REPRESENTATION_RELATIONSHIP( ) );
#3970 = ORIENTED_EDGE ( 'NONE', *, *, #1373, .F. ) ;
#3971 = CARTESIAN_POINT ( 'NONE',  ( -4.147343260682193389, -9.916251082295019614, 22.73823205004162773 ) ) ;
#3972 = CARTESIAN_POINT ( 'NONE',  ( 11.57174281757876955, 8.159736356077653241, 35.66679457777021867 ) ) ;
#3973 = DIRECTION ( 'NONE',  ( -0.9326495259660493309, 0.3607836771741531612, 0.000000000000000000 ) ) ;
#3974 = ORIENTED_EDGE ( 'NONE', *, *, #723, .F. ) ;
#3975 = CARTESIAN_POINT ( 'NONE',  ( 80.08403291566574467, -27.64547812922912939, -79.99999999999998579 ) ) ;
#3976 = CARTESIAN_POINT ( 'NONE',  ( -1.716658579843648003, -9.908812303639328078, 25.63028407385523266 ) ) ;
#3977 = ORIENTED_EDGE ( 'NONE', *, *, #90, .T. ) ;
#3978 = CARTESIAN_POINT ( 'NONE',  ( 74.61196207728411878, -28.86269417393183190, 38.99999999999995737 ) ) ;
#3979 = EDGE_LOOP ( 'NONE', ( #5870, #2684, #919, #5351 ) ) ;
#3980 = CARTESIAN_POINT ( 'NONE',  ( -5.114554293134481958E-14, -6.349488965209747807E-14, -35.00000000000000000 ) ) ;
#3981 = FACE_OUTER_BOUND ( 'NONE', #5169, .T. ) ;
#3982 = ITEM_DEFINED_TRANSFORMATION ( 'NONE', 'NONE', #3938,  #73 ) ;
#3983 = CARTESIAN_POINT ( 'NONE',  ( -72.00000000000004263, 0.000000000000000000, 35.00000000000000000 ) ) ;
#3984 = DIRECTION ( 'NONE',  ( 1.000000000000000000, 0.000000000000000000, 0.000000000000000000 ) ) ;
#3985 = ORIENTED_EDGE ( 'NONE', *, *, #2230, .T. ) ;
#3986 = ADVANCED_FACE ( 'NONE', ( #3235 ), #4099, .F. ) ;
#3987 = ADVANCED_FACE ( 'NONE', ( #1795 ), #6118, .F. ) ;
#3988 = ORIENTED_EDGE ( 'NONE', *, *, #5073, .F. ) ;
#3989 = CARTESIAN_POINT ( 'NONE',  ( 12.00000000000000000, 12.00000000000000355, 20.00000000000000000 ) ) ;
#3990 = CARTESIAN_POINT ( 'NONE',  ( 9.999999999999998224, 6.666666666666638541, 23.00000000000000000 ) ) ;
#3991 = DIRECTION ( 'NONE',  ( 0.000000000000000000, 0.000000000000000000, 1.000000000000000000 ) ) ;
#3992 = ORIENTED_EDGE ( 'NONE', *, *, #5502, .F. ) ;
#3993 = CARTESIAN_POINT ( 'NONE',  ( 0.000000000000000000, 67.50000000000000000, 19.00000000000000000 ) ) ;
#3994 = EDGE_CURVE ( 'NONE', #5424, #816, #3145, .T. ) ;
#3995 = CARTESIAN_POINT ( 'NONE',  ( -12.74240908541723805, -1.902479615894477893, 33.26151609189631841 ) ) ;
#3996 = VERTEX_POINT ( 'NONE', #5604 ) ;
#3997 = CARTESIAN_POINT ( 'NONE',  ( 0.000000000000000000, -67.50000000000000000, 35.00000000000000000 ) ) ;
#3998 = EDGE_CURVE ( 'NONE', #2972, #5395, #3178, .T. ) ;
#3999 = CARTESIAN_POINT ( 'NONE',  ( 9.462636878983097688, 7.610208295502463471, 25.48187184588751464 ) ) ;
#4000 = CARTESIAN_POINT ( 'NONE',  ( 5.141101056459331353, 67.50000000000000000, -19.00000000000000000 ) ) ;
#4001 = VERTEX_POINT ( 'NONE', #4547 ) ;
#4002 = DIRECTION ( 'NONE',  ( -0.000000000000000000, -0.000000000000000000, 1.000000000000000000 ) ) ;
#4003 = CARTESIAN_POINT ( 'NONE',  ( -3.531766105781287468, -10.70751178813581461, 28.15279191876807729 ) ) ;
#4004 = VERTEX_POINT ( 'NONE', #1678 ) ;
#4005 = DIRECTION ( 'NONE',  ( -0.000000000000000000, -0.000000000000000000, 1.000000000000000000 ) ) ;
#4006 = ORIENTED_EDGE ( 'NONE', *, *, #1869, .F. ) ;
#4007 = DIRECTION ( 'NONE',  ( -0.7787725926866162496, 0.6273063437270229858, 0.000000000000000000 ) ) ;
#4008 = PLANE ( 'NONE',  #3739 ) ;
#4009 = PRODUCT_CONTEXT ( 'NONE', #2134, 'mechanical' ) ;
#4010 = DIRECTION ( 'NONE',  ( 0.7787725926866080339, 0.6273063437270329779, 0.000000000000000000 ) ) ;
#4011 = CARTESIAN_POINT ( 'NONE',  ( 9.000000000000005329, -8.999999999988066435, 23.06137295785747554 ) ) ;
#4012 = ORIENTED_EDGE ( 'NONE', *, *, #3198, .F. ) ;
#4013 = ORIENTED_EDGE ( 'NONE', *, *, #5024, .F. ) ;
#4014 = CARTESIAN_POINT ( 'NONE',  ( 0.000000000000000000, 50.91502622129181788, 35.00000000000000000 ) ) ;
#4015 = LINE ( 'NONE', #1651, #4234 ) ;
#4016 = AXIS2_PLACEMENT_3D ( 'NONE', #5915, #3103, #5010 ) ;
#4017 = ORIENTED_EDGE ( 'NONE', *, *, #2367, .T. ) ;
#4018 = DIRECTION ( 'NONE',  ( -0.000000000000000000, -0.000000000000000000, -1.000000000000000000 ) ) ;
#4019 = CARTESIAN_POINT ( 'NONE',  ( -14.21240711833873505, -4.002955306052623285, 38.32637886702301699 ) ) ;
#4020 = VERTEX_POINT ( 'NONE', #1248 ) ;
#4021 = VECTOR ( 'NONE', #4826, 1000.000000000000000 ) ;
#4022 = DIRECTION ( 'NONE',  ( -0.000000000000000000, -0.000000000000000000, 1.000000000000000000 ) ) ;
#4023 = CARTESIAN_POINT ( 'NONE',  ( 85.08403291566575888, -27.64547812922912939, -40.00000000000000000 ) ) ;
#4024 = ADVANCED_FACE ( 'NONE', ( #2735 ), #5143, .T. ) ;
#4025 = AXIS2_PLACEMENT_3D ( 'NONE', #3027, #5436, #5030 ) ;
#4026 = VECTOR ( 'NONE', #6066, 1000.000000000000000 ) ;
#4027 = CARTESIAN_POINT ( 'NONE',  ( 8.963498645742985715, 4.986905650496026965, 23.01829711214647745 ) ) ;
#4028 = ADVANCED_FACE ( 'NONE', ( #2148 ), #2268, .F. ) ;
#4029 = LINE ( 'NONE', #2100, #1539 ) ;
#4030 = ORIENTED_EDGE ( 'NONE', *, *, #2773, .T. ) ;
#4031 = ORIENTED_EDGE ( 'NONE', *, *, #99, .T. ) ;
#4032 = EDGE_CURVE ( 'NONE', #1950, #936, #4605, .T. ) ;
#4033 = VECTOR ( 'NONE', #3219, 1000.000000000000000 ) ;
#4034 = CARTESIAN_POINT ( 'NONE',  ( -0.9505942623812230208, -12.81596724893641515, 33.26667497053199440 ) ) ;
#4035 = ORIENTED_EDGE ( 'NONE', *, *, #4210, .T. ) ;
#4036 = DIRECTION ( 'NONE',  ( 0.000000000000000000, 0.000000000000000000, 1.000000000000000000 ) ) ;
#4037 = VERTEX_POINT ( 'NONE', #5086 ) ;
#4038 = DIRECTION ( 'NONE',  ( 0.000000000000000000, 0.000000000000000000, 1.000000000000000000 ) ) ;
#4039 = CARTESIAN_POINT ( 'NONE',  ( -9.074396217167327805, 58.26942451214400620, -35.00000000000000000 ) ) ;
#4040 = ITEM_DEFINED_TRANSFORMATION ( 'NONE', 'NONE', #4333,  #73 ) ;
#4041 = DIRECTION ( 'NONE',  ( 1.000000000000000000, 0.000000000000000000, 0.000000000000000000 ) ) ;
#4042 = CARTESIAN_POINT ( 'NONE',  ( 9.074396217167167933, 58.26942451214404173, 35.00000000000000000 ) ) ;
#4043 = CIRCLE ( 'NONE', #1180, 80.00000000000000000 ) ;
#4044 = VERTEX_POINT ( 'NONE', #1224 ) ;
#4045 = CARTESIAN_POINT ( 'NONE',  ( 9.419333092093010507, 9.933255351449998827, 30.50691708577705796 ) ) ;
#4046 = DIRECTION ( 'NONE',  ( -0.000000000000000000, -0.000000000000000000, -1.000000000000000000 ) ) ;
#4047 = CYLINDRICAL_SURFACE ( 'NONE', #4839, 12.50000000000138556 ) ;
#4048 = CIRCLE ( 'NONE', #4247, 100.0000000000000000 ) ;
#4049 = ORIENTED_EDGE ( 'NONE', *, *, #3576, .T. ) ;
#4050 = PRODUCT_RELATED_PRODUCT_CATEGORY ( 'part', '', ( #2845 ) ) ;
#4051 = DIRECTION ( 'NONE',  ( 1.000000000000000000, 0.000000000000000000, 0.000000000000000000 ) ) ;
#4052 = CIRCLE ( 'NONE', #2477, 12.49999999999999822 ) ;
#4053 = CARTESIAN_POINT ( 'NONE',  ( -10.46302782743270754, 5.247549479766074221, 28.11481907968152782 ) ) ;
#4054 = CIRCLE ( 'NONE', #1279, 4.999999999999997335 ) ;
#4055 = ORIENTED_EDGE ( 'NONE', *, *, #5309, .T. ) ;
#4056 = CARTESIAN_POINT ( 'NONE',  ( -10.13908112636437053, 9.618700053625529378, 30.46372964425718521 ) ) ;
#4057 = CARTESIAN_POINT ( 'NONE',  ( 12.31015466235579225, -79.04720167209512738, 35.00000000000000000 ) ) ;
#4058 = FILL_AREA_STYLE ('',( #1550 ) ) ;
#4059 = EDGE_CURVE ( 'NONE', #2065, #132, #5723, .T. ) ;
#4060 = ADVANCED_FACE ( 'NONE', ( #2184 ), #4072, .F. ) ;
#4061 = CARTESIAN_POINT ( 'NONE',  ( 46.52501622030217021, 37.47620048660763103, -35.00000000000000000 ) ) ;
#4062 = DIRECTION ( 'NONE',  ( 0.9880900209011890256, 0.1538769332794488465, -0.000000000000000000 ) ) ;
#4063 = VERTEX_POINT ( 'NONE', #2797 ) ;
#4064 = CARTESIAN_POINT ( 'NONE',  ( -9.696021465980070531, 12.35760627049922533, 37.99999999999999289 ) ) ;
#4065 = ADVANCED_FACE ( 'NONE', ( #2398 ), #482, .F. ) ;
#4066 = CARTESIAN_POINT ( 'NONE',  ( -1.955660088736181144E-14, -12.81596724893641515, 33.26667497053200151 ) ) ;
#4067 = EDGE_LOOP ( 'NONE', ( #3850, #590, #173, #2333 ) ) ;
#4068 = CARTESIAN_POINT ( 'NONE',  ( -9.000000000000005329, 8.999999999988014920, 23.06137295785748265 ) ) ;
#4069 = ORIENTED_EDGE ( 'NONE', *, *, #5850, .T. ) ;
#4070 = CARTESIAN_POINT ( 'NONE',  ( -12.00215801354769063, -70.99259259259262933, 35.00000000000000000 ) ) ;
#4071 = DIRECTION ( 'NONE',  ( 1.000000000000000000, 0.000000000000000000, 0.000000000000000000 ) ) ;
#4072 = PLANE ( 'NONE',  #5616 ) ;
#4073 = CARTESIAN_POINT ( 'NONE',  ( -14.79903580929012463, 5.273949241992682779, 38.00000000000001421 ) ) ;
#4074 = ADVANCED_FACE ( 'NONE', ( #3849 ), #4695, .F. ) ;
#4075 = ORIENTED_EDGE ( 'NONE', *, *, #521, .F. ) ;
#4076 = CARTESIAN_POINT ( 'NONE',  ( 14.99999999999995559, -1.301042606982595854E-14, 35.00000000000000000 ) ) ;
#4077 = CARTESIAN_POINT ( 'NONE',  ( 9.999999999999998224, -9.999999999999998224, 23.00000000000000000 ) ) ;
#4078 = B_SPLINE_SURFACE_WITH_KNOTS ( 'NONE', 3, 3, ( 
 ( #539, #57, #1878, #1002, #2417, #1383, #467 ),
 ( #4754, #436, #5755, #4306, #3288, #5660, #5259 ),
 ( #5788, #3773, #5193, #966, #3405, #1416, #1907 ),
 ( #2353, #4243, #6140, #3803, #5718, #1446, #1942 ),
 ( #3348, #1032, #2883, #1481, #3838, #3377, #2911 ),
 ( #5290, #4816, #569, #2789, #250, #2122, #2488 ),
 ( #2067, #5386, #4890, #2515, #1538, #1126, #4914 ),
 ( #4946, #3900, #5411, #1147, #606, #4375, #4403 ),
 ( #4019, #1099, #2606, #125, #1177, #223, #725 ),
 ( #3006, #151, #663, #3968, #5942, #2033, #2980 ),
 ( #4470, #4496, #3995, #3443, #2543, #3934, #5884 ),
 ( #5853, #1063, #4437, #2096, #1600, #1572, #1657 ),
 ( #3474, #3525, #694, #3032, #4857, #192, #5909 ),
 ( #4978, #2576, #5353, #3497, #1622, #5815, #5443 ),
 ( #3069, #638, #5317, #2945, #2005, #402, #2279 ),
 ( #6083, #4171, #2248, #3559, #315, #5005, #3159 ),
 ( #4108, #1233, #3186, #1208, #4525, #4648, #1287 ),
 ( #2662, #2717, #867, #4146, #1687, #1261, #2193 ),
 ( #5095, #4615, #342, #6059, #4053, #2217, #841 ),
 ( #3124, #5972, #4560, #1780, #4084, #6028, #370 ),
 ( #5588, #1749, #3674, #1313, #3214, #3613, #5121 ),
 ( #2750, #3647, #815, #5067, #2691, #5478, #3587 ),
 ( #3098, #5505, #750, #2632, #281, #2158, #5036 ),
 ( #783, #5998, #1712, #5534, #4589, #5563, #1832 ),
 ( #4901, #5613, #4419, #2922, #3914, #5774, #3733 ) ),
 .UNSPECIFIED., .F., .F., .F.,
 ( 4, 3, 3, 3, 3, 3, 3, 3, 4 ),
 ( 4, 3, 4 ),
 ( 0.000000000000000000, 0.1250000000000000000, 0.2500000000000000000, 0.3750000000000000000, 0.5000000000000000000, 0.6250000000000000000, 0.7500000000000000000, 0.8750000000000000000, 1.000000000000000000 ),
 ( 0.000000000000000000, 0.5087255983319458608, 1.017451196663891722 ),
 .UNSPECIFIED. ) ;
#4079 = CARTESIAN_POINT ( 'NONE',  ( -3.314202382262247060, 14.30535051437897742, 38.17196567842750454 ) ) ;
#4080 = CARTESIAN_POINT ( 'NONE',  ( -47.58482424179536707, 72.37680137756343868, -40.00000000000000000 ) ) ;
#4081 = SHAPE_REPRESENTATION ( 'Stationary spindle', ( #73 ), #1747 ) ;
#4082 = ORIENTED_EDGE ( 'NONE', *, *, #2056, .F. ) ;
#4083 = CARTESIAN_POINT ( 'NONE',  ( 8.963498645742985715, -4.986905650496099796, 23.01829711214647745 ) ) ;
#4084 = CARTESIAN_POINT ( 'NONE',  ( -10.32655419438761690, 6.095889600840175504, 28.09296952102860345 ) ) ;
#4085 = EDGE_LOOP ( 'NONE', ( #3339, #5136 ) ) ;
#4086 = DIRECTION ( 'NONE',  ( -1.000000000000000000, 0.000000000000000000, 0.000000000000000000 ) ) ;
#4087 =( NAMED_UNIT ( * ) PLANE_ANGLE_UNIT ( ) SI_UNIT ( $, .RADIAN. ) );
#4088 = CARTESIAN_POINT ( 'NONE',  ( -14.99999999999995559, -1.301042606982600272E-14, 20.00000000000000000 ) ) ;
#4089 = CARTESIAN_POINT ( 'NONE',  ( 12.00000000000000000, 0.000000000000000000, 20.00000000000000000 ) ) ;
#4090 = VERTEX_POINT ( 'NONE', #4729 ) ;
#4091 = EDGE_CURVE ( 'NONE', #4790, #3470, #4620, .T. ) ;
#4092 = CARTESIAN_POINT ( 'NONE',  ( -9.515772848102853843, -10.27564057804868902, 33.05475024408053741 ) ) ;
#4093 = ORIENTED_EDGE ( 'NONE', *, *, #438, .T. ) ;
#4094 = DIRECTION ( 'NONE',  ( -0.000000000000000000, -0.000000000000000000, 1.000000000000000000 ) ) ;
#4095 = ORIENTED_EDGE ( 'NONE', *, *, #4407, .T. ) ;
#4096 = CARTESIAN_POINT ( 'NONE',  ( 2.941541598353386116E-14, -7.604078429494091299E-14, 35.00000000000000000 ) ) ;
#4097 = CARTESIAN_POINT ( 'NONE',  ( 0.000000000000000000, 0.000000000000000000, 205.0000000000000568 ) ) ;
#4098 = EDGE_CURVE ( 'NONE', #2846, #5114, #70, .T. ) ;
#4099 = PLANE ( 'NONE',  #3431 ) ;
#4100 = CARTESIAN_POINT ( 'NONE',  ( -15.67638808697554786, 1.082228759108216254, 38.00000000000000711 ) ) ;
#4101 = DIRECTION ( 'NONE',  ( -0.000000000000000000, 0.000000000000000000, 1.000000000000000000 ) ) ;
#4102 = EDGE_LOOP ( 'NONE', ( #931, #3018, #3662, #1462 ) ) ;
#4103 = CARTESIAN_POINT ( 'NONE',  ( 67.15076586955576943, -25.97642475653856664, 45.00000000000000711 ) ) ;
#4104 = DIRECTION ( 'NONE',  ( -0.000000000000000000, -0.000000000000000000, -1.000000000000000000 ) ) ;
#4105 = CARTESIAN_POINT ( 'NONE',  ( 12.00000000000000000, 50.91502622129181788, 35.00000000000000000 ) ) ;
#4106 = ADVANCED_FACE ( 'NONE', ( #519 ), #2364, .F. ) ;
#4107 = CARTESIAN_POINT ( 'NONE',  ( 11.42336634021359032, -4.532931003857849639, 30.68084270896568810 ) ) ;
#4108 = CARTESIAN_POINT ( 'NONE',  ( -14.21238549857230993, 4.003063095775585722, 38.32638145091770809 ) ) ;
#4109 = ORIENTED_EDGE ( 'NONE', *, *, #181, .F. ) ;
#4110 = CARTESIAN_POINT ( 'NONE',  ( -4.533051537554481314, 11.42333844578497626, 30.68084101284746623 ) ) ;
#4112 = TOROIDAL_SURFACE ( 'NONE', #4016, 72.00000000000004263, 10.00000000000000000 ) ;
#4111 = DIRECTION ( 'NONE',  ( 1.000000000000000000, 0.000000000000000000, 0.000000000000000000 ) ) ;
#4113 = CYLINDRICAL_SURFACE ( 'NONE', #965, 4.999999999999990230 ) ;
#4114 = AXIS2_PLACEMENT_3D ( 'NONE', #2580, #2162, #2664 ) ;
#4115 = AXIS2_PLACEMENT_3D ( 'NONE', #3813, #36, #2423 ) ;
#4116 = DIRECTION ( 'NONE',  ( -0.000000000000000000, 0.000000000000000000, 1.000000000000000000 ) ) ;
#4117 = AXIS2_PLACEMENT_3D ( 'NONE', #3750, #2795, #3321 ) ;
#4118 = DIRECTION ( 'NONE',  ( -0.1538769332794488187, 0.9880900209011889146, 0.000000000000000000 ) ) ;
#4119 = MANIFOLD_SOLID_BREP ( 'Shell1', #1755 ) ;
#4120 = AXIS2_PLACEMENT_3D ( 'NONE', #2627, #3520, #5475 ) ;
#4121 = CIRCLE ( 'NONE', #5129, 80.00000000000000000 ) ;
#4122 = UNCERTAINTY_MEASURE_WITH_UNIT (LENGTH_MEASURE( 1.000000000000000082E-05 ), #2307, 'distance_accuracy_value', 'NONE');
#4123 = VECTOR ( 'NONE', #1549, 1000.000000000000000 ) ;
#4124 = PRODUCT_RELATED_PRODUCT_CATEGORY ( 'part', '', ( #970 ) ) ;
#4125 = PRODUCT ( 'tube', 'tube', '', ( #768 ) ) ;
#4126 = CARTESIAN_POINT ( 'NONE',  ( 0.000000000000000000, 0.000000000000000000, -40.00000000000000000 ) ) ;
#4127 = AXIS2_PLACEMENT_3D ( 'NONE', #2901, #2837, #3890 ) ;
#4128 = ORIENTED_EDGE ( 'NONE', *, *, #2593, .F. ) ;
#4129 = CARTESIAN_POINT ( 'NONE',  ( 54.99999999999975131, 21.27605460800048576, 35.00000000000000000 ) ) ;
#4130 = ORIENTED_EDGE ( 'NONE', *, *, #4793, .T. ) ;
#4131 = DIRECTION ( 'NONE',  ( 1.000000000000000000, 0.000000000000000000, 0.000000000000000000 ) ) ;
#4132 = VECTOR ( 'NONE', #3082, 1000.000000000000000 ) ;
#4133 = DIRECTION ( 'NONE',  ( -1.000000000000000000, 0.000000000000000000, 0.000000000000000000 ) ) ;
#4134 = LINE ( 'NONE', #4162, #1541 ) ;
#4135 = CARTESIAN_POINT ( 'NONE',  ( 14.99999999999995559, -1.301042606982595854E-14, 35.00000000000000000 ) ) ;
#4136 = DIRECTION ( 'NONE',  ( -0.000000000000000000, -0.000000000000000000, -1.000000000000000000 ) ) ;
#4137 = EDGE_CURVE ( 'NONE', #506, #2123, #4668, .T. ) ;
#4138 = EDGE_CURVE ( 'NONE', #1185, #2223, #1066, .T. ) ;
#4139 = ORIENTED_EDGE ( 'NONE', *, *, #3170, .T. ) ;
#4140 = CARTESIAN_POINT ( 'NONE',  ( -5.000000000000003553, 89.46264649666795776, -40.00000000000000000 ) ) ;
#4141 = LINE ( 'NONE', #2776, #2540 ) ;
#4142 = CARTESIAN_POINT ( 'NONE',  ( -9.676903716103852915, 11.04476983075539565, 38.07288907902119490 ) ) ;
#4143 = CARTESIAN_POINT ( 'NONE',  ( 11.85339260696609465, -0.9193131588476518568, 30.72304697887226510 ) ) ;
#4144 = VECTOR ( 'NONE', #809, 1000.000000000000000 ) ;
#4145 = EDGE_CURVE ( 'NONE', #5444, #1288, #4187, .T. ) ;
#4146 = CARTESIAN_POINT ( 'NONE',  ( -11.42336634021359387, 4.532931003857847863, 30.68084270896569521 ) ) ;
#4147 = ORIENTED_EDGE ( 'NONE', *, *, #3994, .F. ) ;
#4148 = CARTESIAN_POINT ( 'NONE',  ( -2.654236408786703194, 10.78034266696900012, 28.16346921039841078 ) ) ;
#4149 = CARTESIAN_POINT ( 'NONE',  ( -12.31015466235495026, -79.04720167209526949, 38.99999999999995737 ) ) ;
#4150 = CARTESIAN_POINT ( 'NONE',  ( 0.000000000000000000, 0.000000000000000000, 38.99999999999995737 ) ) ;
#4151 = CIRCLE ( 'NONE', #1181, 14.67638808697554964 ) ;
#4152 = DIRECTION ( 'NONE',  ( 0.000000000000000000, 0.000000000000000000, 1.000000000000000000 ) ) ;
#4153 = VECTOR ( 'NONE', #3889, 1000.000000000000000 ) ;
#4154 = DIRECTION ( 'NONE',  ( -0.000000000000000000, -0.000000000000000000, -1.000000000000000000 ) ) ;
#4155 = AXIS2_PLACEMENT_3D ( 'NONE', #2799, #5173, #4697 ) ;
#4156 = CARTESIAN_POINT ( 'NONE',  ( -8.432825516645550579, -9.370308891928099015, 25.44727539999420074 ) ) ;
#4157 = ORIENTED_EDGE ( 'NONE', *, *, #1322, .T. ) ;
#4158 = CARTESIAN_POINT ( 'NONE',  ( 11.33314185117008677, -72.77350886804093477, -35.00000000000000000 ) ) ;
#4159 = ORIENTED_EDGE ( 'NONE', *, *, #6093, .T. ) ;
#4160 = DIRECTION ( 'NONE',  ( -1.000000000000000000, 0.000000000000000000, 0.000000000000000000 ) ) ;
#4161 = CARTESIAN_POINT ( 'NONE',  ( 55.00000000000024158, -21.27605460799916770, -35.00000000000000000 ) ) ;
#4162 = CARTESIAN_POINT ( 'NONE',  ( 0.000000000000000000, 50.91502622129181788, 20.00000000000000000 ) ) ;
#4163 = CARTESIAN_POINT ( 'NONE',  ( -9.999999999999998224, -0.8333333333332838544, 23.00000000000000000 ) ) ;
#4164 = CARTESIAN_POINT ( 'NONE',  ( 0.000000000000000000, 0.000000000000000000, -35.00000000000000000 ) ) ;
#4165 = ORIENTED_EDGE ( 'NONE', *, *, #4457, .F. ) ;
#4166 = CARTESIAN_POINT ( 'NONE',  ( 0.000000000000000000, 9.999999999999998224, 20.00000000000000000 ) ) ;
#4167 = DIRECTION ( 'NONE',  ( -0.000000000000000000, 0.000000000000000000, 1.000000000000000000 ) ) ;
#4168 = CARTESIAN_POINT ( 'NONE',  ( -55.71784976887214924, 21.55374571496067304, 35.00000000000000000 ) ) ;
#4169 = ADVANCED_FACE ( 'NONE', ( #3781 ), #1394, .F. ) ;
#4170 = CARTESIAN_POINT ( 'NONE',  ( 9.928243323025451872, -0.8581648076837659067, 25.63579099555280649 ) ) ;
#4171 = CARTESIAN_POINT ( 'NONE',  ( -13.51119013911331024, 2.923529524533194923, 35.79437308157104525 ) ) ;
#4172 = VERTEX_POINT ( 'NONE', #1424 ) ;
#4173 = CARTESIAN_POINT ( 'NONE',  ( -1.839621235173124703, 11.79778917763282209, 30.71783072571432882 ) ) ;
#4174 = CARTESIAN_POINT ( 'NONE',  ( 12.00215801354769063, 70.99259259259262933, 35.00000000000000000 ) ) ;
#4175 = ADVANCED_FACE ( 'NONE', ( #1458 ), #5635, .F. ) ;
#4176 = EDGE_LOOP ( 'NONE', ( #2814, #5535, #3291, #636, #3977, #2754, #3140, #489, #242, #3611 ) ) ;
#4177 = CARTESIAN_POINT ( 'NONE',  ( 0.000000000000000000, 0.000000000000000000, 35.00000000000000000 ) ) ;
#4178 = PLANE ( 'NONE',  #3632 ) ;
#4179 = DIRECTION ( 'NONE',  ( -0.7787725926866080339, -0.6273063437270329779, 0.000000000000000000 ) ) ;
#4180 = EDGE_CURVE ( 'NONE', #5932, #3300, #3296, .T. ) ;
#4181 = CARTESIAN_POINT ( 'NONE',  ( -9.245260337044127752, -9.269614772507658529, 25.40693856330804934 ) ) ;
#4182 = ORIENTED_EDGE ( 'NONE', *, *, #2118, .T. ) ;
#4183 = DIRECTION ( 'NONE',  ( 0.000000000000000000, 1.000000000000000000, 0.000000000000000000 ) ) ;
#4184 = ORIENTED_EDGE ( 'NONE', *, *, #1399, .T. ) ;
#4185 = DIRECTION ( 'NONE',  ( -0.000000000000000000, 0.000000000000000000, 1.000000000000000000 ) ) ;
#4186 = CYLINDRICAL_SURFACE ( 'NONE', #2965, 12.50000000000138556 ) ;
#4187 = LINE ( 'NONE', #3717, #3924 ) ;
#4188 = EDGE_LOOP ( 'NONE', ( #4082, #3614, #2399, #257 ) ) ;
#4189 = CARTESIAN_POINT ( 'NONE',  ( -9.916251082295017838, -4.147343260682107235, 22.73823205004162418 ) ) ;
#4190 = CARTESIAN_POINT ( 'NONE',  ( -80.00000000000000000, 0.000000000000000000, 40.00000000000000000 ) ) ;
#4191 = ORIENTED_EDGE ( 'NONE', *, *, #253, .F. ) ;
#4192 = CARTESIAN_POINT ( 'NONE',  ( -68.69027832784050247, 26.57196568621489163, 35.00000000000000000 ) ) ;
#4193 = LINE ( 'NONE', #6108, #1927 ) ;
#4194 = CARTESIAN_POINT ( 'NONE',  ( 4.735139425640385369, 13.92517021172140446, 38.16137691020119860 ) ) ;
#4195 = CARTESIAN_POINT ( 'NONE',  ( 13.51119013911330846, -2.923529524533198476, 35.79437308157105235 ) ) ;
#4196 = MANIFOLD_SOLID_BREP ( 'Fillet1', #2459 ) ;
#4197 = DIRECTION ( 'NONE',  ( 0.000000000000000000, 0.000000000000000000, 1.000000000000000000 ) ) ;
#4198 = ORIENTED_EDGE ( 'NONE', *, *, #1323, .F. ) ;
#4199 = CARTESIAN_POINT ( 'NONE',  ( -4.986905650496027853, 8.963498645742985715, 23.01829711214647745 ) ) ;
#4200 = VERTEX_POINT ( 'NONE', #5365 ) ;
#4201 = DIRECTION ( 'NONE',  ( 1.000000000000000000, 0.000000000000000000, 0.000000000000000000 ) ) ;
#4202 = ORIENTED_EDGE ( 'NONE', *, *, #1847, .T. ) ;
#4203 = DIRECTION ( 'NONE',  ( 1.000000000000000000, 0.000000000000000000, 0.000000000000000000 ) ) ;
#4204 = DIRECTION ( 'NONE',  ( -0.000000000000000000, 0.000000000000000000, -1.000000000000000000 ) ) ;
#4205 = VECTOR ( 'NONE', #4552, 1000.000000000000000 ) ;
#4206 = EDGE_CURVE ( 'NONE', #4976, #3788, #2548, .T. ) ;
#4207 = DIRECTION ( 'NONE',  ( -0.000000000000000000, 0.000000000000000000, 1.000000000000000000 ) ) ;
#4208 = AXIS2_PLACEMENT_3D ( 'NONE', #3167, #5077, #348 ) ;
#4209 = CARTESIAN_POINT ( 'NONE',  ( 12.31015466235495204, 79.04720167209528370, -35.00000000000000711 ) ) ;
#4210 = EDGE_CURVE ( 'NONE', #429, #3444, #361, .T. ) ;
#4211 = VERTEX_POINT ( 'NONE', #5977 ) ;
#4212 = CARTESIAN_POINT ( 'NONE',  ( 9.192833548570215285, 59.02994620157096506, -35.00000000000000000 ) ) ;
#4213 = CIRCLE ( 'NONE', #3229, 10.00000000000000000 ) ;
#4214 = VERTEX_POINT ( 'NONE', #5797 ) ;
#4215 = DIRECTION ( 'NONE',  ( -0.4999999999999920619, -0.8660254037844432595, 0.000000000000000000 ) ) ;
#4216 = AXIS2_PLACEMENT_3D ( 'NONE', #4566, #2014, #1986 ) ;
#4217 = DIRECTION ( 'NONE',  ( -0.000000000000000000, -0.000000000000000000, -1.000000000000000000 ) ) ;
#4218 = VECTOR ( 'NONE', #2361, 1000.000000000000000 ) ;
#4219 = PRESENTATION_STYLE_ASSIGNMENT (( #2327 ) ) ;
#4220 = ORIENTED_EDGE ( 'NONE', *, *, #1485, .F. ) ;
#4221 = PLANE ( 'NONE',  #2873 ) ;
#4222 = CIRCLE ( 'NONE', #969, 72.00000000000004263 ) ;
#4223 = LINE ( 'NONE', #4190, #5063 ) ;
#4224 = VECTOR ( 'NONE', #1294, 1000.000000000000000 ) ;
#4225 = ORIENTED_EDGE ( 'NONE', *, *, #2665, .F. ) ;
#4226 = ORIENTED_EDGE ( 'NONE', *, *, #2520, .T. ) ;
#4227 = CARTESIAN_POINT ( 'NONE',  ( 52.58482424179643289, 72.37680137756268550, -40.00000000000000000 ) ) ;
#4228 = DIRECTION ( 'NONE',  ( 1.000000000000000000, -5.329070518200750605E-15, 0.000000000000000000 ) ) ;
#4229 = AXIS2_PLACEMENT_3D ( 'NONE', #5308, #4741, #951 ) ;
#4230 = DIRECTION ( 'NONE',  ( 0.000000000000000000, -0.000000000000000000, -1.000000000000000000 ) ) ;
#4231 = VECTOR ( 'NONE', #4786, 1000.000000000000000 ) ;
#4232 = CYLINDRICAL_SURFACE ( 'NONE', #4972, 5.000000000000004441 ) ;
#4233 = ORIENTED_EDGE ( 'NONE', *, *, #3275, .T. ) ;
#4234 = VECTOR ( 'NONE', #274, 1000.000000000000000 ) ;
#4235 = CARTESIAN_POINT ( 'NONE',  ( -4.954970571217796937, 13.90079966151758128, 38.30990426830500439 ) ) ;
#4236 = B_SPLINE_CURVE_WITH_KNOTS ( 'NONE', 3,
 ( #671, #133, #5917, #1632, #5454, #1186 ),
 .UNSPECIFIED., .F., .F.,
 ( 4, 2, 4 ),
 ( 0.002357188415687188742, 0.01135824717474478128, 0.02035930593380237338 ),
 .UNSPECIFIED. ) ;
#4237 = EDGE_LOOP ( 'NONE', ( #3988, #5618, #1658, #1379, #152 ) ) ;
#4238 = DIRECTION ( 'NONE',  ( -0.000000000000000000, -0.000000000000000000, -1.000000000000000000 ) ) ;
#4239 = EDGE_CURVE ( 'NONE', #2445, #730, #163, .T. ) ;
#4240 = ORIENTED_EDGE ( 'NONE', *, *, #4677, .F. ) ;
#4241 = DIRECTION ( 'NONE',  ( -1.000000000000000000, 0.000000000000000000, 0.000000000000000000 ) ) ;
#4242 = CIRCLE ( 'NONE', #598, 11.50000000000000355 ) ;
#4243 = CARTESIAN_POINT ( 'NONE',  ( -11.57174281757876599, -8.159736356077647912, 35.66679457777020446 ) ) ;
#4244 = AXIS2_PLACEMENT_3D ( 'NONE', #5557, #5148, #2713 ) ;
#4245 = DIRECTION ( 'NONE',  ( -0.5000000000000038858, 0.8660254037844362651, 0.000000000000000000 ) ) ;
#4246 = UNCERTAINTY_MEASURE_WITH_UNIT (LENGTH_MEASURE( 1.000000000000000082E-05 ), #1819, 'distance_accuracy_value', 'NONE');
#4247 = AXIS2_PLACEMENT_3D ( 'NONE', #448, #890, #2237 ) ;
#4248 = EDGE_CURVE ( 'NONE', #3364, #1302, #1715, .T. ) ;
#4249 = EDGE_CURVE ( 'NONE', #906, #1548, #571, .T. ) ;
#4250 = AXIS2_PLACEMENT_3D ( 'NONE', #883, #831, #800 ) ;
#4251 = VECTOR ( 'NONE', #3425, 999.9999999999998863 ) ;
#4252 = LINE ( 'NONE', #5321, #2764 ) ;
#4253 = ORIENTED_EDGE ( 'NONE', *, *, #2397, .F. ) ;
#4254 = DIRECTION ( 'NONE',  ( 0.000000000000000000, 0.000000000000000000, 1.000000000000000000 ) ) ;
#4255 = CONICAL_SURFACE ( 'NONE', #398, 99.00000000000005684, 0.7853981633974552734 ) ;
#4256 = ORIENTED_EDGE ( 'NONE', *, *, #4893, .F. ) ;
#4257 = CARTESIAN_POINT ( 'NONE',  ( -8.999999999999998224, 0.000000000000000000, -167.0000000000000284 ) ) ;
#4258 = DIRECTION ( 'NONE',  ( 8.673617379884026597E-16, -1.000000000000000000, 0.000000000000000000 ) ) ;
#4259 = ORIENTED_EDGE ( 'NONE', *, *, #1188, .T. ) ;
#4260 = EDGE_CURVE ( 'NONE', #2151, #5943, #3438, .T. ) ;
#4261 = CARTESIAN_POINT ( 'NONE',  ( 14.55721289103181348, -1.928061058260302607, 38.18004976450265531 ) ) ;
#4262 = AXIS2_PLACEMENT_3D ( 'NONE', #1868, #83, #3863 ) ;
#4263 = CARTESIAN_POINT ( 'NONE',  ( 4.533051537554480426, -11.42333844578497448, 30.68084101284746978 ) ) ;
#4264 = ORIENTED_EDGE ( 'NONE', *, *, #2517, .F. ) ;
#4265 = ORIENTED_EDGE ( 'NONE', *, *, #1777, .T. ) ;
#4266 = DIRECTION ( 'NONE',  ( 0.000000000000000000, -0.000000000000000000, 1.000000000000000000 ) ) ;
#4267 = DIRECTION ( 'NONE',  ( -0.9326495259660420034, -0.3607836771741717574, 0.000000000000000000 ) ) ;
#4268 = CARTESIAN_POINT ( 'NONE',  ( 0.000000000000000000, 0.000000000000000000, 0.000000000000000000 ) ) ;
#4269 = CARTESIAN_POINT ( 'NONE',  ( 0.000000000000000000, 67.50000000000000000, 20.00000000000000000 ) ) ;
#4270 = EDGE_CURVE ( 'NONE', #5854, #5996, #4545, .T. ) ;
#4271 = CYLINDRICAL_SURFACE ( 'NONE', #611, 12.50000000000139266 ) ;
#4272 = VERTEX_POINT ( 'NONE', #3944 ) ;
#4273 = CARTESIAN_POINT ( 'NONE',  ( 4.954793796408216267, 13.90087379555094849, 38.30989703917857270 ) ) ;
#4274 = PRODUCT_DEFINITION_SHAPE ( 'NONE', 'NONE',  #6141 ) ;
#4275 = CARTESIAN_POINT ( 'NONE',  ( 6.666666666666693608, 9.999999999999998224, 23.00000000000000000 ) ) ;
#4276 = CARTESIAN_POINT ( 'NONE',  ( -80.00000000000000000, 0.000000000000000000, -35.00000000000000000 ) ) ;
#4277 = ORIENTED_EDGE ( 'NONE', *, *, #5766, .F. ) ;
#4278 = LINE ( 'NONE', #29, #456 ) ;
#4279 = CARTESIAN_POINT ( 'NONE',  ( 80.00000000000000000, 0.000000000000000000, 38.99999999999995737 ) ) ;
#4280 =( REPRESENTATION_RELATIONSHIP ('NONE','NONE', #4716, #82 ) REPRESENTATION_RELATIONSHIP_WITH_TRANSFORMATION ( #3054 )SHAPE_REPRESENTATION_RELATIONSHIP( ) );
#4281 = CARTESIAN_POINT ( 'NONE',  ( 9.269614772507654976, 9.245260337044125976, 25.40693856330804223 ) ) ;
#4282 = DIRECTION ( 'NONE',  ( 1.000000000000000000, 0.000000000000000000, 0.000000000000000000 ) ) ;
#4283 = VERTEX_POINT ( 'NONE', #4353 ) ;
#4284 = CARTESIAN_POINT ( 'NONE',  ( -9.074396217167167933, -58.26942451214404173, 35.00000000000000000 ) ) ;
#4285 = ADVANCED_FACE ( 'NONE', ( #1583 ), #5829, .F. ) ;
#4286 = DIRECTION ( 'NONE',  ( -0.000000000000000000, -0.000000000000000000, -1.000000000000000000 ) ) ;
#4287 = CARTESIAN_POINT ( 'NONE',  ( -7.182140071210238271E-14, 8.916303653273167033E-14, 35.00000000000000000 ) ) ;
#4288 = ORIENTED_EDGE ( 'NONE', *, *, #5954, .T. ) ;
#4289 = FACE_OUTER_BOUND ( 'NONE', #2992, .T. ) ;
#4290 = CARTESIAN_POINT ( 'NONE',  ( 7.869812776064875948, -10.50531938289192624, 30.57803900350706527 ) ) ;
#4291 = ORIENTED_EDGE ( 'NONE', *, *, #3247, .T. ) ;
#4292 = ORIENTED_EDGE ( 'NONE', *, *, #2892, .T. ) ;
#4293 = CARTESIAN_POINT ( 'NONE',  ( -52.58482424179695158, -72.37680137756228760, -40.00000000000000000 ) ) ;
#4294 = ADVANCED_FACE ( 'NONE', ( #286 ), #2988, .F. ) ;
#4295 = CARTESIAN_POINT ( 'NONE',  ( 0.000000000000000000, 0.000000000000000000, -20.00000000000000000 ) ) ;
#4296 = CYLINDRICAL_SURFACE ( 'NONE', #790, 4.999999999999997335 ) ;
#4297 = CARTESIAN_POINT ( 'NONE',  ( -85.08403291566554572, 27.64547812922971914, -79.99999999999998579 ) ) ;
#4298 = CARTESIAN_POINT ( 'NONE',  ( 10.12138240269938549, -10.27356722921338950, 35.55812462721154787 ) ) ;
#4299 = VERTEX_POINT ( 'NONE', #1041 ) ;
#4300 = EDGE_CURVE ( 'NONE', #3800, #6084, #4923, .T. ) ;
#4301 = CARTESIAN_POINT ( 'NONE',  ( 3.879012780925822579, 13.33504572891042272, 35.78373437249953781 ) ) ;
#4302 = CARTESIAN_POINT ( 'NONE',  ( 9.166666666666673180, 9.999999999999998224, 23.00000000000000000 ) ) ;
#4303 = DIRECTION ( 'NONE',  ( 1.000000000000000000, 0.000000000000000000, 0.000000000000000000 ) ) ;
#4304 = EDGE_LOOP ( 'NONE', ( #4556, #1421, #4735, #692, #1967 ) ) ;
#4305 = CARTESIAN_POINT ( 'NONE',  ( 0.000000000000000000, 12.00000000000000355, 35.00000000000000000 ) ) ;
#4306 = CARTESIAN_POINT ( 'NONE',  ( -9.933255351449995274, -9.419333092093001625, 30.50691708577705086 ) ) ;
#4307 = CARTESIAN_POINT ( 'NONE',  ( 5.141101056459331353, 67.50000000000000000, 28.99999999999999645 ) ) ;
#4308 = UNCERTAINTY_MEASURE_WITH_UNIT (LENGTH_MEASURE( 1.000000000000000082E-05 ), #2245, 'distance_accuracy_value', 'NONE');
#4309 = TOROIDAL_SURFACE ( 'NONE', #5120, 72.00000000000004263, 10.00000000000000000 ) ;
#4310 = CARTESIAN_POINT ( 'NONE',  ( 10.38144361273100635, 10.38144361273100635, 38.10175261887127363 ) ) ;
#4311 = CARTESIAN_POINT ( 'NONE',  ( -7.356224370873720275, -12.70872189800991059, 38.12480727770462607 ) ) ;
#4312 = VERTEX_POINT ( 'NONE', #106 ) ;
#4313 = DIRECTION ( 'NONE',  ( -0.000000000000000000, -0.000000000000000000, -1.000000000000000000 ) ) ;
#4314 = PLANE ( 'NONE',  #886 ) ;
#4315 = CIRCLE ( 'NONE', #3709, 55.00000000000001421 ) ;
#4316 = CARTESIAN_POINT ( 'NONE',  ( -1.594625153350711036E-14, -1.594625153350706303E-14, 20.00000000000000000 ) ) ;
#4317 = ORIENTED_EDGE ( 'NONE', *, *, #1979, .F. ) ;
#4318 = CARTESIAN_POINT ( 'NONE',  ( 5.000000000000003553, 89.46264649666795776, 40.00000000000000000 ) ) ;
#4319 = CARTESIAN_POINT ( 'NONE',  ( 3.322926169935022322, -8.964120776013638547, 23.06129021161081383 ) ) ;
#4320 = CIRCLE ( 'NONE', #270, 5.000000000000004441 ) ;
#4321 = EDGE_LOOP ( 'NONE', ( #3253, #5752, #4930, #2264, #5951, #384 ) ) ;
#4322 = DIRECTION ( 'NONE',  ( 0.4999999999999980016, 0.8660254037844398178, 0.000000000000000000 ) ) ;
#4323 = ORIENTED_EDGE ( 'NONE', *, *, #961, .F. ) ;
#4324 = CARTESIAN_POINT ( 'NONE',  ( -11.50000000000000178, 67.50000000000000000, -20.00000000000000000 ) ) ;
#4325 = CARTESIAN_POINT ( 'NONE',  ( 45.92560378283280187, 36.99336990414421678, 35.00000000000000000 ) ) ;
#4326 = DIRECTION ( 'NONE',  ( -0.000000000000000000, -0.000000000000000000, -1.000000000000000000 ) ) ;
#4327 = CARTESIAN_POINT ( 'NONE',  ( -12.74932535096585262, 83.41975492014094584, 0.000000000000000000 ) ) ;
#4328 = AXIS2_PLACEMENT_3D ( 'NONE', #220, #1684, #5969 ) ;
#4329 = DIRECTION ( 'NONE',  ( -1.000000000000000000, 0.000000000000000000, 0.000000000000000000 ) ) ;
#4330 = CARTESIAN_POINT ( 'NONE',  ( 12.11088206474084394, -8.328520801854338629, 38.20782360758020246 ) ) ;
#4331 = EDGE_CURVE ( 'NONE', #3160, #1611, #2314, .T. ) ;
#4332 = ADVANCED_FACE ( 'NONE', ( #2350 ), #4113, .F. ) ;
#4333 = AXIS2_PLACEMENT_3D ( 'NONE', #3396, #2023, #1962 ) ;
#4334 = ORIENTED_EDGE ( 'NONE', *, *, #1885, .F. ) ;
#4335 = CARTESIAN_POINT ( 'NONE',  ( 0.9833031778629314212, 13.77854189090673742, 35.81030296219172726 ) ) ;
#4336 = CARTESIAN_POINT ( 'NONE',  ( -4.260267006495014996, 15.12434353048566571, 38.00000000000000711 ) ) ;
#4337 = CARTESIAN_POINT ( 'NONE',  ( -68.69027832784050247, 26.57196568621489163, 35.13717928826310555 ) ) ;
#4338 = ORIENTED_EDGE ( 'NONE', *, *, #128, .T. ) ;
#4339 = EDGE_CURVE ( 'NONE', #1288, #5804, #2732, .T. ) ;
#4340 = DIRECTION ( 'NONE',  ( 0.4999999999999979461, 0.8660254037844397068, 0.000000000000000000 ) ) ;
#4341 = EDGE_CURVE ( 'NONE', #1931, #4450, #1069, .T. ) ;
#4342 = PLANE ( 'NONE',  #1263 ) ;
#4343 = CARTESIAN_POINT ( 'NONE',  ( 5.809855716632613465, -9.930636381741159369, 22.73823205004162773 ) ) ;
#4344 = ADVANCED_FACE ( 'NONE', ( #1841 ), #3652, .T. ) ;
#4345 = DIRECTION ( 'NONE',  ( -0.000000000000000000, -0.000000000000000000, -1.000000000000000000 ) ) ;
#4346 = VECTOR ( 'NONE', #3295, 1000.000000000000000 ) ;
#4347 = CARTESIAN_POINT ( 'NONE',  ( 10.03503361918882320, -10.72051346006293571, 38.06197354439399305 ) ) ;
#4348 = ORIENTED_EDGE ( 'NONE', *, *, #5828, .T. ) ;
#4349 = CARTESIAN_POINT ( 'NONE',  ( -67.48246767247867695, 25.10212255632726297, 35.00000000000000000 ) ) ;
#4350 = CARTESIAN_POINT ( 'NONE',  ( -68.69027832783800136, -26.57196568621473531, 35.00000000000000000 ) ) ;
#4351 = VECTOR ( 'NONE', #2523, 1000.000000000000000 ) ;
#4352 = VECTOR ( 'NONE', #4007, 999.9999999999998863 ) ;
#4353 = CARTESIAN_POINT ( 'NONE',  ( -55.71784976887420271, -21.55374571496209057, 35.00000000000000000 ) ) ;
#4354 = ORIENTED_EDGE ( 'NONE', *, *, #5072, .F. ) ;
#4355 = DIRECTION ( 'NONE',  ( -0.000000000000000000, -0.000000000000000000, -1.000000000000000000 ) ) ;
#4356 = CARTESIAN_POINT ( 'NONE',  ( 7.732441893382014264, -9.977717576970368540, 28.03187055541259909 ) ) ;
#4357 = VERTEX_POINT ( 'NONE', #5659 ) ;
#4358 = SURFACE_STYLE_FILL_AREA ( #6113 ) ;
#4359 = ORIENTED_EDGE ( 'NONE', *, *, #3266, .T. ) ;
#4360 = DIRECTION ( 'NONE',  ( 0.000000000000000000, 0.000000000000000000, 1.000000000000000000 ) ) ;
#4361 = DIRECTION ( 'NONE',  ( -1.000000000000000000, 0.000000000000000000, 0.000000000000000000 ) ) ;
#4362 = DIRECTION ( 'NONE',  ( 1.000000000000000000, 0.000000000000000000, 0.000000000000000000 ) ) ;
#4363 = DIRECTION ( 'NONE',  ( 1.665334536937734811E-16, -1.000000000000000222, 2.150297872858148760E-18 ) ) ;
#4364 = AXIS2_PLACEMENT_3D ( 'NONE', #4905, #2111, #2084 ) ;
#4365 = LINE ( 'NONE', #1590, #2770 ) ;
#4366 = CARTESIAN_POINT ( 'NONE',  ( 8.975362584346067152, -9.157688896001753065, 22.85246612729342885 ) ) ;
#4367 = ORIENTED_EDGE ( 'NONE', *, *, #248, .F. ) ;
#4368 = EDGE_LOOP ( 'NONE', ( #1239, #5607, #1530, #2589 ) ) ;
#4369 = CARTESIAN_POINT ( 'NONE',  ( -1.660911000355770772, 8.965240827029074211, 23.08598180255751942 ) ) ;
#4370 = CARTESIAN_POINT ( 'NONE',  ( 9.981067540164714202, 9.981067540164714202, 22.73823205004162418 ) ) ;
#4371 = CARTESIAN_POINT ( 'NONE',  ( -14.58318388806637778, -1.909955344851256065, 38.18050947768618641 ) ) ;
#4372 = ADVANCED_FACE ( 'NONE', ( #1809 ), #1265, .T. ) ;
#4373 = ORIENTED_EDGE ( 'NONE', *, *, #4916, .T. ) ;
#4374 = LINE ( 'NONE', #568, #5432 ) ;
#4375 = CARTESIAN_POINT ( 'NONE',  ( -9.778265433844637755, -4.273103006804783277, 25.59105575288735324 ) ) ;
#4376 = EDGE_LOOP ( 'NONE', ( #6043, #3208, #1522, #1171, #2858 ) ) ;
#4377 = DIRECTION ( 'NONE',  ( -0.000000000000000000, -0.000000000000000000, -1.000000000000000000 ) ) ;
#4378 = ADVANCED_FACE ( 'NONE', ( #2787 ), #6090, .T. ) ;
#4379 = CARTESIAN_POINT ( 'NONE',  ( 14.21240711833874037, 4.002955306052626838, 38.32637886702303121 ) ) ;
#4380 = DIRECTION ( 'NONE',  ( 0.6273063437270329779, -0.7787725926866080339, 0.000000000000000000 ) ) ;
#4381 = EDGE_LOOP ( 'NONE', ( #2977, #4017 ) ) ;
#4382 = DIRECTION ( 'NONE',  ( -0.000000000000000000, -0.000000000000000000, -1.000000000000000000 ) ) ;
#4383 = EDGE_CURVE ( 'NONE', #37, #4784, #5333, .T. ) ;
#4384 = PLANE ( 'NONE',  #5651 ) ;
#4385 = CARTESIAN_POINT ( 'NONE',  ( 11.33314185116896589, 72.77350886803867525, 35.13717928826270054 ) ) ;
#4386 = VERTEX_POINT ( 'NONE', #4684 ) ;
#4387 = LINE ( 'NONE', #5919, #2174 ) ;
#4388 = CARTESIAN_POINT ( 'NONE',  ( 5.113933401365476250, -9.708537589994012507, 25.56820946177495912 ) ) ;
#4389 = ORIENTED_EDGE ( 'NONE', *, *, #1901, .T. ) ;
#4390 = DIRECTION ( 'NONE',  ( 0.000000000000000000, 0.000000000000000000, 1.000000000000000000 ) ) ;
#4391 = ORIENTED_EDGE ( 'NONE', *, *, #3414, .F. ) ;
#4392 = DIRECTION ( 'NONE',  ( -4.496403249731883200E-15, 1.000000000000000000, 0.000000000000000000 ) ) ;
#4393 = DIRECTION ( 'NONE',  ( 0.000000000000000000, 0.000000000000000000, 1.000000000000000000 ) ) ;
#4394 = CARTESIAN_POINT ( 'NONE',  ( 0.000000000000000000, 0.000000000000000000, 0.000000000000000000 ) ) ;
#4395 = DIRECTION ( 'NONE',  ( -0.000000000000000000, -0.000000000000000000, 1.000000000000000000 ) ) ;
#4396 = DIRECTION ( 'NONE',  ( 0.000000000000000000, 0.000000000000000000, 1.000000000000000000 ) ) ;
#4397 = ORIENTED_EDGE ( 'NONE', *, *, #2311, .F. ) ;
#4398 = CARTESIAN_POINT ( 'NONE',  ( 1.589281154371899412E-14, 12.81596724893641515, 33.26667497053200151 ) ) ;
#4399 = CARTESIAN_POINT ( 'NONE',  ( -4.166666666666626107, 9.999999999999998224, 23.00000000000000000 ) ) ;
#4400 = DIRECTION ( 'NONE',  ( 1.000000000000000000, 0.000000000000000000, 0.000000000000000000 ) ) ;
#4401 = ORIENTED_EDGE ( 'NONE', *, *, #2935, .T. ) ;
#4402 = CARTESIAN_POINT ( 'NONE',  ( -58.45671475544946816, -33.75000000000027711, 35.00000000000000000 ) ) ;
#4403 = CARTESIAN_POINT ( 'NONE',  ( -8.963431230391419646, -4.154428044945158938, 23.04275563843252783 ) ) ;
#4404 = APPLICATION_CONTEXT ( 'automotive_design' ) ;
#4405 = VERTEX_POINT ( 'NONE', #1382 ) ;
#4406 = CARTESIAN_POINT ( 'NONE',  ( 2.164213882025729951, -15.56315586465741951, 38.00000000000000711 ) ) ;
#4407 = EDGE_CURVE ( 'NONE', #4299, #993, #4320, .T. ) ;
#4408 = EDGE_CURVE ( 'NONE', #413, #2346, #3818, .T. ) ;
#4409 = CARTESIAN_POINT ( 'NONE',  ( 10.32656711695237739, 6.095798759547078838, 28.09297316833070113 ) ) ;
#4410 = DIRECTION ( 'NONE',  ( -0.000000000000000000, -0.000000000000000000, -1.000000000000000000 ) ) ;
#4411 = ORIENTED_EDGE ( 'NONE', *, *, #4727, .T. ) ;
#4412 = CARTESIAN_POINT ( 'NONE',  ( -11.99999999999999645, 12.00000000000000355, 20.00000000000000000 ) ) ;
#4413 = CARTESIAN_POINT ( 'NONE',  ( -52.58482424179695158, -72.37680137756228760, 40.00000000000000000 ) ) ;
#4414 = ADVANCED_FACE ( 'NONE', ( #874 ), #376, .F. ) ;
#4415 = ADVANCED_FACE ( 'NONE', ( #5619 ), #3164, .F. ) ;
#4416 = CIRCLE ( 'NONE', #2342, 80.00000000000000000 ) ;
#4417 = CARTESIAN_POINT ( 'NONE',  ( 1.839621235173124036, -11.79778917763282386, 30.71783072571433237 ) ) ;
#4418 = ORIENTED_EDGE ( 'NONE', *, *, #2780, .F. ) ;
#4419 = CARTESIAN_POINT ( 'NONE',  ( -9.858401829237468661, 10.19494410001831142, 33.01259202755186095 ) ) ;
#4420 = CIRCLE ( 'NONE', #954, 12.50000000000000178 ) ;
#4421 = ORIENTED_EDGE ( 'NONE', *, *, #787, .T. ) ;
#4422 = DIRECTION ( 'NONE',  ( 0.000000000000000000, 0.000000000000000000, 1.000000000000000000 ) ) ;
#4423 = CARTESIAN_POINT ( 'NONE',  ( -90.08403291566554572, 27.64547812922971914, -79.99999999999998579 ) ) ;
#4424 = ITEM_DEFINED_TRANSFORMATION ( 'NONE', 'NONE', #2948,  #73 ) ;
#4425 = CARTESIAN_POINT ( 'NONE',  ( -5.000000000000629718, -89.46264649666795776, 40.00000000000000000 ) ) ;
#4426 = DIRECTION ( 'NONE',  ( -0.000000000000000000, -0.000000000000000000, 1.000000000000000000 ) ) ;
#4427 = AXIS2_PLACEMENT_3D ( 'NONE', #4795, #3323, #4766 ) ;
#4428 = VECTOR ( 'NONE', #1392, 1000.000000000000000 ) ;
#4429 = ORIENTED_EDGE ( 'NONE', *, *, #2015, .F. ) ;
#4430 = CARTESIAN_POINT ( 'NONE',  ( 7.869812776064898152, 10.50531938289192802, 30.57803900350706527 ) ) ;
#4431 = CARTESIAN_POINT ( 'NONE',  ( 10.00000000000000000, 0.8333333333332849646, 23.00000000000000355 ) ) ;
#4433 = AXIS2_PLACEMENT_3D ( 'NONE', #3312, #2384, #6033 ) ;
#4432 = DIRECTION ( 'NONE',  ( -0.000000000000000000, -0.000000000000000000, -1.000000000000000000 ) ) ;
#4434 = AXIS2_PLACEMENT_3D ( 'NONE', #4177, #3287, #5074 ) ;
#4435 = ORIENTED_EDGE ( 'NONE', *, *, #5626, .T. ) ;
#4436 = FACE_OUTER_BOUND ( 'NONE', #199, .T. ) ;
#4437 = CARTESIAN_POINT ( 'NONE',  ( -12.81596724893641337, -0.9505942623811892700, 33.26667497053200151 ) ) ;
#4438 = ORIENTED_EDGE ( 'NONE', *, *, #1629, .T. ) ;
#4439 = CARTESIAN_POINT ( 'NONE',  ( -4.260267006495018549, -15.12434353048566571, 38.00000000000000711 ) ) ;
#4440 = CIRCLE ( 'NONE', #5140, 100.0000000000000000 ) ;
#4441 = CARTESIAN_POINT ( 'NONE',  ( 10.85316926984840791, 1.776762854451773510, 28.17414535953233923 ) ) ;
#4442 = ORIENTED_EDGE ( 'NONE', *, *, #946, .T. ) ;
#4443 = CARTESIAN_POINT ( 'NONE',  ( -55.48030965893044453, 45.89047003626346566, 35.00000000000000000 ) ) ;
#4444 = VECTOR ( 'NONE', #339, 1000.000000000000114 ) ;
#4445 = EDGE_CURVE ( 'NONE', #4784, #6084, #1754, .T. ) ;
#4446 = EDGE_CURVE ( 'NONE', #2223, #3051, #4121, .T. ) ;
#4447 = CARTESIAN_POINT ( 'NONE',  ( -68.69027832783800136, -26.57196568621473531, 35.13717928826270054 ) ) ;
#4448 = AXIS2_PLACEMENT_3D ( 'NONE', #134, #4866, #618 ) ;
#4449 = CARTESIAN_POINT ( 'NONE',  ( -3.577867169202164632E-15, -14.74111653287705792, 38.35393095385146012 ) ) ;
#4450 = VERTEX_POINT ( 'NONE', #845 ) ;
#4451 = CARTESIAN_POINT ( 'NONE',  ( 0.000000000000000000, 67.50000000000000000, -20.00000000000000000 ) ) ;
#4452 = ORIENTED_EDGE ( 'NONE', *, *, #3282, .F. ) ;
#4453 = CARTESIAN_POINT ( 'NONE',  ( -1.630640067418198669E-13, 67.50000000000002842, 35.00000000000000000 ) ) ;
#4454 = DIRECTION ( 'NONE',  ( -0.000000000000000000, 0.000000000000000000, 1.000000000000000000 ) ) ;
#4455 = DIRECTION ( 'NONE',  ( 0.000000000000000000, 0.000000000000000000, 1.000000000000000000 ) ) ;
#4456 = CIRCLE ( 'NONE', #2575, 5.141101056459331353 ) ;
#4457 = EDGE_CURVE ( 'NONE', #4357, #1548, #2721, .T. ) ;
#4458 = DIRECTION ( 'NONE',  ( 1.000000000000000000, 0.000000000000000000, 0.000000000000000000 ) ) ;
#4459 = CARTESIAN_POINT ( 'NONE',  ( 12.00000000000000000, 12.00000000000000355, 35.00000000000000000 ) ) ;
#4460 = AXIS2_PLACEMENT_3D ( 'NONE', #4126, #1760, #3659 ) ;
#4461 = EDGE_LOOP ( 'NONE', ( #1219, #4833 ) ) ;
#4462 = FACE_OUTER_BOUND ( 'NONE', #2513, .T. ) ;
#4463 = CIRCLE ( 'NONE', #3657, 12.50000000000138911 ) ;
#4464 = CARTESIAN_POINT ( 'NONE',  ( 11.73806315776973541, -10.43169748385511042, 38.00000000000000711 ) ) ;
#4465 = CARTESIAN_POINT ( 'NONE',  ( 7.182140071210238271E-14, -8.916303653273167033E-14, 35.00000000000000000 ) ) ;
#4466 = EDGE_CURVE ( 'NONE', #2239, #5444, #1445, .T. ) ;
#4467 = VERTEX_POINT ( 'NONE', #3314 ) ;
#4468 = DIRECTION ( 'NONE',  ( -0.9326495259660445569, -0.3607836771741652071, 0.000000000000000000 ) ) ;
#4469 = B_SPLINE_CURVE_WITH_KNOTS ( 'NONE', 3,
 ( #2143, #2731, #5959, #4577 ),
 .UNSPECIFIED., .F., .F.,
 ( 4, 4 ),
 ( 0.000000000000000000, 0.001907370850886561109 ),
 .UNSPECIFIED. ) ;
#4470 = CARTESIAN_POINT ( 'NONE',  ( -14.63232105816060802, -2.035738251814319000, 38.34842656511671066 ) ) ;
#4471 = VERTEX_POINT ( 'NONE', #1939 ) ;
#4472 = FACE_BOUND ( 'NONE', #4705, .T. ) ;
#4473 = CARTESIAN_POINT ( 'NONE',  ( 13.07368784376655135, 4.807938790076512703, 35.76776929191790089 ) ) ;
#4474 = DIRECTION ( 'NONE',  ( -0.1538769332794418798, 0.9880900209011901358, 0.000000000000000000 ) ) ;
#4475 = ORIENTED_EDGE ( 'NONE', *, *, #138, .T. ) ;
#4476 = DIRECTION ( 'NONE',  ( -1.000000000000000000, 0.000000000000000000, 0.000000000000000000 ) ) ;
#4477 = CARTESIAN_POINT ( 'NONE',  ( 11.07913919611939058, 71.14248150488579370, 45.00000000000000711 ) ) ;
#4478 = CARTESIAN_POINT ( 'NONE',  ( -2.742560498089771315, -11.69030472852371005, 30.70728637550628903 ) ) ;
#4479 = ORIENTED_EDGE ( 'NONE', *, *, #3998, .F. ) ;
#4480 = DIRECTION ( 'NONE',  ( 0.000000000000000000, -1.000000000000000000, 0.000000000000000000 ) ) ;
#4481 = ORIENTED_EDGE ( 'NONE', *, *, #4759, .F. ) ;
#4482 = CARTESIAN_POINT ( 'NONE',  ( 0.000000000000000000, 0.000000000000000000, 35.00000000000000000 ) ) ;
#4483 = FACE_OUTER_BOUND ( 'NONE', #1837, .T. ) ;
#4484 = APPLICATION_PROTOCOL_DEFINITION ( 'draft international standard', 'automotive_design', 1998, #5128 ) ;
#4485 = DIRECTION ( 'NONE',  ( -0.000000000000000000, -0.000000000000000000, -1.000000000000000000 ) ) ;
#4486 = DIRECTION ( 'NONE',  ( -0.000000000000000000, -0.000000000000000000, -1.000000000000000000 ) ) ;
#4487 = ORIENTED_EDGE ( 'NONE', *, *, #1487, .T. ) ;
#4488 = ADVANCED_FACE ( 'NONE', ( #3404 ), #3772, .F. ) ;
#4489 = ORIENTED_EDGE ( 'NONE', *, *, #2970, .F. ) ;
#4490 = CARTESIAN_POINT ( 'NONE',  ( 7.228600378928579318, 11.39263409468387245, 33.15620577507543487 ) ) ;
#4491 = CARTESIAN_POINT ( 'NONE',  ( 9.900940235153615987, -0.8289898103094419657, 22.73823205004162418 ) ) ;
#4492 = FACE_OUTER_BOUND ( 'NONE', #5974, .T. ) ;
#4493 = EDGE_LOOP ( 'NONE', ( #4883, #5523, #3830, #5288, #5050, #2598, #2628, #2043, #3134, #3363 ) ) ;
#4494 = FACE_OUTER_BOUND ( 'NONE', #1045, .T. ) ;
#4495 = EDGE_CURVE ( 'NONE', #4527, #5114, #5729, .T. ) ;
#4496 = CARTESIAN_POINT ( 'NONE',  ( -13.68731696136523368, -1.968147360634810106, 35.80501325620552677 ) ) ;
#4497 = EDGE_LOOP ( 'NONE', ( #5069, #2700, #4721, #4348, #622 ) ) ;
#4498 = CARTESIAN_POINT ( 'NONE',  ( -9.632247231687287581, 10.63625351335941893, 35.59852902770369099 ) ) ;
#4499 = DIRECTION ( 'NONE',  ( 1.000000000000000000, 0.000000000000000000, 0.000000000000000000 ) ) ;
#4500 = CARTESIAN_POINT ( 'NONE',  ( 11.98089146579572706, 5.533593864557656339, 33.20390238845318720 ) ) ;
#4501 = LINE ( 'NONE', #5949, #570 ) ;
#4502 = EDGE_LOOP ( 'NONE', ( #6139, #938 ) ) ;
#4503 = ORIENTED_EDGE ( 'NONE', *, *, #4260, .F. ) ;
#4504 = CARTESIAN_POINT ( 'NONE',  ( -5.845970755595367052, -13.50805179034378511, 38.28811402100272687 ) ) ;
#4505 = ORIENTED_EDGE ( 'NONE', *, *, #4206, .T. ) ;
#4506 = DIRECTION ( 'NONE',  ( 0.000000000000000000, 1.000000000000000000, 0.000000000000000000 ) ) ;
#4507 = ORIENTED_EDGE ( 'NONE', *, *, #3494, .F. ) ;
#4508 = LINE ( 'NONE', #2021, #891 ) ;
#4509 = ADVANCED_FACE ( 'NONE', ( #637 ), #4815, .F. ) ;
#4510 = DIRECTION ( 'NONE',  ( 0.7787725926866080339, 0.6273063437270329779, 0.000000000000000000 ) ) ;
#4511 = CONTEXT_DEPENDENT_SHAPE_REPRESENTATION ( #2586, #167 ) ;
#4512 = DIRECTION ( 'NONE',  ( -0.9880900209011910240, 0.1538769332794358846, 0.000000000000000000 ) ) ;
#4513 = DIRECTION ( 'NONE',  ( 0.000000000000000000, 0.000000000000000000, 1.000000000000000000 ) ) ;
#4514 = VECTOR ( 'NONE', #3554, 1000.000000000000000 ) ;
#4515 = EDGE_LOOP ( 'NONE', ( #352, #784, #3894, #1977 ) ) ;
#4516 = CARTESIAN_POINT ( 'NONE',  ( 8.007183658747752730, 11.03292118881348749, 33.12420745160152791 ) ) ;
#4517 = CARTESIAN_POINT ( 'NONE',  ( 9.999999999999998224, -1.666666666666713814, 23.00000000000000000 ) ) ;
#4518 = DIRECTION ( 'NONE',  ( -0.6273063437270329779, 0.7787725926866080339, 0.000000000000000000 ) ) ;
#4519 = CIRCLE ( 'NONE', #58, 12.50000000000138911 ) ;
#4520 = EDGE_CURVE ( 'NONE', #1681, #5256, #2942, .T. ) ;
#4521 = PRESENTATION_LAYER_ASSIGNMENT (  '', '', ( #59 ) ) ;
#4522 = EDGE_CURVE ( 'NONE', #5096, #3527, #4623, .T. ) ;
#4523 = VERTEX_POINT ( 'NONE', #5688 ) ;
#4524 = CARTESIAN_POINT ( 'NONE',  ( -2.941541598353333735E-14, 7.604078429494112756E-14, 35.00000000000000000 ) ) ;
#4525 = CARTESIAN_POINT ( 'NONE',  ( -10.70751178813581284, 3.531766105781286580, 28.15279191876807374 ) ) ;
#4526 = CIRCLE ( 'NONE', #1634, 5.000000000000005329 ) ;
#4527 = VERTEX_POINT ( 'NONE', #963 ) ;
#4528 = VECTOR ( 'NONE', #5716, 1000.000000000000000 ) ;
#4529 = FACE_OUTER_BOUND ( 'NONE', #2386, .T. ) ;
#4530 = PLANE ( 'NONE',  #6024 ) ;
#4531 = EDGE_CURVE ( 'NONE', #1185, #4450, #3441, .T. ) ;
#4532 = CARTESIAN_POINT ( 'NONE',  ( -2.941541598353333735E-14, 7.604078429494112756E-14, -35.00000000000000000 ) ) ;
#4533 = PRODUCT_DEFINITION_FORMATION_WITH_SPECIFIED_SOURCE ( 'ANY', '', #4125, .NOT_KNOWN. ) ;
#4534 = DIRECTION ( 'NONE',  ( -0.000000000000000000, 0.000000000000000000, 1.000000000000000000 ) ) ;
#4535 = ORIENTED_EDGE ( 'NONE', *, *, #4210, .F. ) ;
#4536 = CARTESIAN_POINT ( 'NONE',  ( -5.833333333333301063, 9.999999999999998224, 23.00000000000000000 ) ) ;
#4537 = AXIS2_PLACEMENT_3D ( 'NONE', #4451, #2763, #2793 ) ;
#4538 = EDGE_CURVE ( 'NONE', #5582, #5277, #4374, .T. ) ;
#4539 = CARTESIAN_POINT ( 'NONE',  ( 2.491918585145396214, -8.964680801521357267, 23.07363600708416840 ) ) ;
#4540 = ORIENTED_EDGE ( 'NONE', *, *, #164, .T. ) ;
#4541 = DIRECTION ( 'NONE',  ( 0.000000000000000000, -0.000000000000000000, 1.000000000000000000 ) ) ;
#4542 = ORIENTED_EDGE ( 'NONE', *, *, #3885, .F. ) ;
#4543 = DIRECTION ( 'NONE',  ( 0.7787725926866080339, 0.6273063437270329779, 0.000000000000000000 ) ) ;
#4544 = LINE ( 'NONE', #300, #2756 ) ;
#4545 = B_SPLINE_CURVE_WITH_KNOTS ( 'NONE', 3,
 ( #3416, #135, #1690, #4385 ),
 .UNSPECIFIED., .F., .F.,
 ( 4, 4 ),
 ( 0.000000000000000000, 0.001907370850883695563 ),
 .UNSPECIFIED. ) ;
#4546 = CIRCLE ( 'NONE', #5451, 5.000000000000005329 ) ;
#4547 = CARTESIAN_POINT ( 'NONE',  ( -62.30180741492871022, -50.18450749816254586, -35.00000000000000000 ) ) ;
#4548 = COLOUR_RGB ( '',0.7921568627450980005, 0.8196078431372548767, 0.9333333333333333481 ) ;
#4549 = CARTESIAN_POINT ( 'NONE',  ( -9.999999999999998224, -6.666666666666634988, 23.00000000000000000 ) ) ;
#4550 = ORIENTED_EDGE ( 'NONE', *, *, #4650, .T. ) ;
#4551 = DIRECTION ( 'NONE',  ( 1.000000000000000000, 0.000000000000000000, 0.000000000000000000 ) ) ;
#4552 = DIRECTION ( 'NONE',  ( -0.000000000000000000, -0.000000000000000000, 1.000000000000000000 ) ) ;
#4553 = CARTESIAN_POINT ( 'NONE',  ( 9.999999999999998224, 4.166666666666626107, 23.00000000000000000 ) ) ;
#4554 = CARTESIAN_POINT ( 'NONE',  ( -5.000000000000629718, -89.46264649666795776, -40.00000000000000000 ) ) ;
#4555 = CIRCLE ( 'NONE', #1859, 80.00000000000000000 ) ;
#4556 = ORIENTED_EDGE ( 'NONE', *, *, #5458, .T. ) ;
#4557 = CARTESIAN_POINT ( 'NONE',  ( 10.46302782743270576, -5.247549479766075109, 28.11481907968152427 ) ) ;
#4558 = AXIS2_PLACEMENT_3D ( 'NONE', #4227, #5675, #1960 ) ;
#4559 = AXIS2_PLACEMENT_3D ( 'NONE', #3367, #1022, #1525 ) ;
#4560 = CARTESIAN_POINT ( 'NONE',  ( -11.71455171164206988, 6.400535080091636075, 33.18278799730943263 ) ) ;
#4561 = CONICAL_SURFACE ( 'NONE', #305, 11.50000000000000355, 0.7853981633974509435 ) ;
#4562 = ORIENTED_EDGE ( 'NONE', *, *, #2284, .F. ) ;
#4563 = CARTESIAN_POINT ( 'NONE',  ( -9.515772848102846737, 10.27564057804868725, 33.05475024408053741 ) ) ;
#4564 = EDGE_CURVE ( 'NONE', #3836, #4690, #3232, .T. ) ;
#4565 = CARTESIAN_POINT ( 'NONE',  ( 15.00000000000000000, 50.91502622129181788, 20.00000000000000000 ) ) ;
#4566 = CARTESIAN_POINT ( 'NONE',  ( 0.000000000000000000, 0.000000000000000000, -35.00000000000000000 ) ) ;
#4567 = AXIS2_PLACEMENT_3D ( 'NONE', #674, #3505, #230 ) ;
#4568 = DIRECTION ( 'NONE',  ( 0.9326495259660445569, 0.3607836771741652626, 0.000000000000000000 ) ) ;
#4569 = ADVANCED_FACE ( 'NONE', ( #3899 ), #5621, .F. ) ;
#4570 = FACE_OUTER_BOUND ( 'NONE', #1938, .T. ) ;
#4571 = ORIENTED_EDGE ( 'NONE', *, *, #1928, .T. ) ;
#4572 = CARTESIAN_POINT ( 'NONE',  ( -8.007183658747754507, -11.03292118881348749, 33.12420745160152791 ) ) ;
#4573 = EDGE_CURVE ( 'NONE', #4952, #6052, #3422, .T. ) ;
#4574 = EDGE_LOOP ( 'NONE', ( #263, #3320, #4202, #5299 ) ) ;
#4575 = CARTESIAN_POINT ( 'NONE',  ( 8.999999999999998224, 0.000000000000000000, -167.0000000000000284 ) ) ;
#4576 = ORIENTED_EDGE ( 'NONE', *, *, #2852, .T. ) ;
#4577 = CARTESIAN_POINT ( 'NONE',  ( 12.00215801354989154, -70.99259259259225985, 35.00000000000000000 ) ) ;
#4578 = DIRECTION ( 'NONE',  ( 1.154631945610162802E-14, -1.000000000000000000, 0.000000000000000000 ) ) ;
#4579 = CONTEXT_DEPENDENT_SHAPE_REPRESENTATION ( #1005, #13 ) ;
#4580 = DIRECTION ( 'NONE',  ( -0.1538769332794358846, -0.9880900209011910240, 0.000000000000000000 ) ) ;
#4581 = CARTESIAN_POINT ( 'NONE',  ( -9.900940235153615987, 0.8289898103094429649, 22.73823205004162418 ) ) ;
#4582 = DIRECTION ( 'NONE',  ( 1.000000000000000000, 0.000000000000000000, 0.000000000000000000 ) ) ;
#4583 = ORIENTED_EDGE ( 'NONE', *, *, #5221, .T. ) ;
#4584 = DIRECTION ( 'NONE',  ( 1.000000000000000000, 0.000000000000000000, 0.000000000000000000 ) ) ;
#4585 = CARTESIAN_POINT ( 'NONE',  ( -12.00000000000000000, 50.91502622129181788, 20.00000000000000000 ) ) ;
#4586 = B_SPLINE_SURFACE_WITH_KNOTS ( 'NONE', 3, 1, ( 
 ( #1417, #1879, #5226 ),
 ( #1484, #1067, #1978 ),
 ( #1103, #2519, #129 ),
 ( #3839, #2007, #2982 ),
 ( #2912, #5758, #4343 ),
 ( #2451, #3902, #4892 ),
 ( #5388, #5818, #640 ),
 ( #4406, #3408, #4918 ),
 ( #665, #5319, #2070 ),
 ( #4859, #2546, #3378 ),
 ( #153, #5291, #2037 ),
 ( #4439, #2418, #194 ),
 ( #3937, #5855, #3971 ),
 ( #3476, #2947, #1033 ),
 ( #5886, #1003, #3349 ),
 ( #1128, #610, #4817 ),
 ( #3008, #572, #5262 ),
 ( #1576, #2490, #1542 ) ),
 .UNSPECIFIED., .F., .F., .F.,
 ( 4, 2, 2, 2, 2, 2, 2, 2, 4 ),
 ( 2, 1, 2 ),
 ( 0.000000000000000000, 0.1250000000000000000, 0.2500000000000000000, 0.3750000000000000000, 0.5000000000000000000, 0.6250000000000000000, 0.7500000000000000000, 0.8750000000000000000, 1.000000000000000000 ),
 ( 0.000000000000000000, 1.000000000000000000, 1.017451196663891499 ),
 .UNSPECIFIED. ) ;
#4587 = SURFACE_SIDE_STYLE ('',( #2687 ) ) ;
#4588 = CARTESIAN_POINT ( 'NONE',  ( 10.32655419438761690, -6.095889600840178169, 28.09296952102860701 ) ) ;
#4589 = CARTESIAN_POINT ( 'NONE',  ( -9.590870124851306855, 9.322893336083163618, 27.95908392747358917 ) ) ;
#4590 = ORIENTED_EDGE ( 'NONE', *, *, #4793, .F. ) ;
#4591 = CARTESIAN_POINT ( 'NONE',  ( -5.113933401365456710, 9.708537589994000072, 25.56820946177495557 ) ) ;
#4592 = DIRECTION ( 'NONE',  ( 0.000000000000000000, -0.000000000000000000, 1.000000000000000000 ) ) ;
#4593 = CARTESIAN_POINT ( 'NONE',  ( 0.000000000000000000, 67.50000000000000000, 19.00000000000000000 ) ) ;
#4594 = CARTESIAN_POINT ( 'NONE',  ( 0.000000000000000000, 50.91502622129181788, -20.00000000000000000 ) ) ;
#4595 = PLANE ( 'NONE',  #5326 ) ;
#4596 = ORIENTED_EDGE ( 'NONE', *, *, #5954, .F. ) ;
#4597 = EDGE_CURVE ( 'NONE', #1798, #2346, #538, .T. ) ;
#4598 = EDGE_CURVE ( 'NONE', #4357, #4988, #3128, .T. ) ;
#4599 = CARTESIAN_POINT ( 'NONE',  ( -10.38144361273100813, -10.38144361273100458, 38.10175261887127363 ) ) ;
#4600 = ORIENTED_EDGE ( 'NONE', *, *, #401, .F. ) ;
#4601 = DIRECTION ( 'NONE',  ( 0.7787725926866080339, 0.6273063437270329779, 0.000000000000000000 ) ) ;
#4602 = EDGE_LOOP ( 'NONE', ( #5105, #221, #4590, #5354, #4696, #1437 ) ) ;
#4603 = LINE ( 'NONE', #4096, #5467 ) ;
#4604 = DIRECTION ( 'NONE',  ( 0.000000000000000000, 1.000000000000000000, 0.000000000000000000 ) ) ;
#4605 = LINE ( 'NONE', #303, #766 ) ;
#4606 = ADVANCED_FACE ( 'NONE', ( #999 ), #2416, .T. ) ;
#4607 = B_SPLINE_CURVE_WITH_KNOTS ( 'NONE', 3,
 ( #1456, #5170, #5270, #975 ),
 .UNSPECIFIED., .F., .F.,
 ( 4, 4 ),
 ( 0.000000000000000000, 0.001907370850886568915 ),
 .UNSPECIFIED. ) ;
#4608 = FACE_OUTER_BOUND ( 'NONE', #3979, .T. ) ;
#4609 = CARTESIAN_POINT ( 'NONE',  ( -52.58482424179536707, 72.37680137756343868, 40.00000000000000000 ) ) ;
#4610 = EDGE_LOOP ( 'NONE', ( #419, #5251, #3630, #5360 ) ) ;
#4611 = CARTESIAN_POINT ( 'NONE',  ( 52.91502622129182498, 15.00000000000001954, 35.00000000000000000 ) ) ;
#4612 = LINE ( 'NONE', #2242, #3521 ) ;
#4613 = CARTESIAN_POINT ( 'NONE',  ( 6.512188664277434924, 13.16119478149493993, 38.13833290264204834 ) ) ;
#4614 = CARTESIAN_POINT ( 'NONE',  ( 8.965668681055127820, -5.138611361899592999E-14, 23.09216300389308785 ) ) ;
#4615 = CARTESIAN_POINT ( 'NONE',  ( -12.74411457810409587, 5.685785403169732355, 35.74643938915853880 ) ) ;
#4616 = ORIENTED_EDGE ( 'NONE', *, *, #2781, .F. ) ;
#4617 = CARTESIAN_POINT ( 'NONE',  ( -2.570253631893256951, 9.871311131128940985, 25.61911440830482789 ) ) ;
#4619 = AXIS2_PLACEMENT_3D ( 'NONE', #5777, #5941, #1499 ) ;
#4618 = CARTESIAN_POINT ( 'NONE',  ( 80.99999999999998579, 9.919639073093559622E-15, -40.00000000000000000 ) ) ;
#4620 = CIRCLE ( 'NONE', #4427, 99.00000000000000000 ) ;
#4621 = DIRECTION ( 'NONE',  ( 0.000000000000000000, 0.000000000000000000, 1.000000000000000000 ) ) ;
#4622 = CIRCLE ( 'NONE', #1068, 10.00000000000000000 ) ;
#4623 = CIRCLE ( 'NONE', #3826, 9.999999999999998224 ) ;
#4624 = ADVANCED_FACE ( 'NONE', ( #4889 ), #92, .F. ) ;
#4625 = CARTESIAN_POINT ( 'NONE',  ( -0.000000000000000000, 9.999999999999998224, -20.00000000000000000 ) ) ;
#4626 = DIRECTION ( 'NONE',  ( 0.000000000000000000, 0.000000000000000000, 1.000000000000000000 ) ) ;
#4627 = AXIS2_PLACEMENT_3D ( 'NONE', #2938, #660, #1121 ) ;
#4628 = CIRCLE ( 'NONE', #68, 4.999999999999997335 ) ;
#4629 = AXIS2_PLACEMENT_3D ( 'NONE', #5076, #4152, #877 ) ;
#4630 = CARTESIAN_POINT ( 'NONE',  ( -9.772747244158502156, -10.99573437649350183, 38.14042781937035187 ) ) ;
#4631 = PRODUCT_DEFINITION_FORMATION_WITH_SPECIFIED_SOURCE ( 'ANY', '', #970, .NOT_KNOWN. ) ;
#4632 = ORIENTED_EDGE ( 'NONE', *, *, #6122, .T. ) ;
#4633 = DIRECTION ( 'NONE',  ( 1.000000000000000000, 0.000000000000000000, 0.000000000000000000 ) ) ;
#4634 = ORIENTED_EDGE ( 'NONE', *, *, #1266, .F. ) ;
#4635 = CARTESIAN_POINT ( 'NONE',  ( 0.000000000000000000, 0.000000000000000000, 38.99999999999995737 ) ) ;
#4636 = EDGE_CURVE ( 'NONE', #5346, #2846, #4278, .T. ) ;
#4637 = DIRECTION ( 'NONE',  ( 1.000000000000000000, 0.000000000000000000, 0.000000000000000000 ) ) ;
#4638 = DIRECTION ( 'NONE',  ( 1.000000000000000000, 8.673617379884027583E-15, 0.000000000000000000 ) ) ;
#4639 = CARTESIAN_POINT ( 'NONE',  ( -9.910574073276151807, -3.317157231508557569, 22.73823205004162418 ) ) ;
#4640 = CARTESIAN_POINT ( 'NONE',  ( -47.58482424179536707, 72.37680137756343868, 40.00000000000000000 ) ) ;
#4641 = ORIENTED_EDGE ( 'NONE', *, *, #793, .F. ) ;
#4642 = DIRECTION ( 'NONE',  ( 0.000000000000000000, -0.000000000000000000, 1.000000000000000000 ) ) ;
#4643 = EDGE_CURVE ( 'NONE', #3297, #559, #1906, .T. ) ;
#4644 = DIRECTION ( 'NONE',  ( -0.000000000000000000, -0.000000000000000000, 1.000000000000000000 ) ) ;
#4645 = DIRECTION ( 'NONE',  ( -0.7787725926866080339, -0.6273063437270329779, 0.000000000000000000 ) ) ;
#4646 = CARTESIAN_POINT ( 'NONE',  ( 8.965668681055129596, 0.8304760625348918124, 23.09216300389309140 ) ) ;
#4647 = AXIS2_PLACEMENT_3D ( 'NONE', #1275, #4604, #5141 ) ;
#4648 = CARTESIAN_POINT ( 'NONE',  ( -9.833809958618568103, 3.423848683943055971, 25.60794474275442667 ) ) ;
#4649 = ORIENTED_EDGE ( 'NONE', *, *, #3873, .F. ) ;
#4650 = EDGE_CURVE ( 'NONE', #328, #2411, #3516, .T. ) ;
#4651 = CARTESIAN_POINT ( 'NONE',  ( -7.393143600131252491, 12.01612071878465393, 35.69844150329612376 ) ) ;
#4652 = AXIS2_PLACEMENT_3D ( 'NONE', #3410, #5322, #614 ) ;
#4653 = CARTESIAN_POINT ( 'NONE',  ( -12.00215801354769063, -70.99259259259262933, 35.00000000000000000 ) ) ;
#4654 = VECTOR ( 'NONE', #1430, 1000.000000000000000 ) ;
#4655 = EDGE_LOOP ( 'NONE', ( #2663, #5868, #1710, #3746 ) ) ;
#4656 = DIRECTION ( 'NONE',  ( 0.7787725926866119197, -0.6273063437270283149, 0.000000000000000000 ) ) ;
#4657 = VECTOR ( 'NONE', #5265, 1000.000000000000000 ) ;
#4658 = DIRECTION ( 'NONE',  ( 1.000000000000000000, 0.000000000000000000, 0.000000000000000000 ) ) ;
#4659 = CIRCLE ( 'NONE', #1973, 12.49999999999999822 ) ;
#4660 = CARTESIAN_POINT ( 'NONE',  ( -6.247143215332724651E-13, -89.46264649666795776, -40.00000000000000000 ) ) ;
#4661 = AXIS2_PLACEMENT_3D ( 'NONE', #1925, #5780, #2996 ) ;
#4662 = CARTESIAN_POINT ( 'NONE',  ( -6.652784304366590185, -8.964415574088988592, 22.96342341013487243 ) ) ;
#4663 = ORIENTED_EDGE ( 'NONE', *, *, #3439, .F. ) ;
#4664 = CARTESIAN_POINT ( 'NONE',  ( 0.000000000000000000, 67.50000000000000000, -20.00000000000000000 ) ) ;
#4665 = ORIENTED_EDGE ( 'NONE', *, *, #5035, .T. ) ;
#4666 = DIRECTION ( 'NONE',  ( 0.000000000000000000, 0.000000000000000000, 1.000000000000000000 ) ) ;
#4667 = DIRECTION ( 'NONE',  ( 1.000000000000000000, 0.000000000000000000, 0.000000000000000000 ) ) ;
#4668 = LINE ( 'NONE', #5731, #3522 ) ;
#4669 = EDGE_LOOP ( 'NONE', ( #4030, #4888 ) ) ;
#4670 = CARTESIAN_POINT ( 'NONE',  ( -9.958856949317492990, -8.309552794738944925, 22.73823205004162418 ) ) ;
#4671 = CARTESIAN_POINT ( 'NONE',  ( 2.941541598353386116E-14, -7.604078429494091299E-14, 35.00000000000000000 ) ) ;
#4672 = VERTEX_POINT ( 'NONE', #2630 ) ;
#4673 = LINE ( 'NONE', #4192, #5358 ) ;
#4674 = CARTESIAN_POINT ( 'NONE',  ( -85.08403291566554572, 27.64547812922971914, -79.99999999999998579 ) ) ;
#4675 = DIRECTION ( 'NONE',  ( -0.000000000000000000, -0.000000000000000000, -1.000000000000000000 ) ) ;
#4676 = CARTESIAN_POINT ( 'NONE',  ( 10.89081796499576882, 0.8880320553140124140, 28.17941898721253580 ) ) ;
#4677 = EDGE_CURVE ( 'NONE', #1473, #705, #5034, .T. ) ;
#4678 = DIRECTION ( 'NONE',  ( 1.000000000000000000, 0.000000000000000000, 0.000000000000000000 ) ) ;
#4679 = ORIENTED_EDGE ( 'NONE', *, *, #1633, .F. ) ;
#4680 = CARTESIAN_POINT ( 'NONE',  ( -7.077301327650770801, 10.77711034800893053, 30.61076202992614270 ) ) ;
#4681 = FACE_OUTER_BOUND ( 'NONE', #2881, .T. ) ;
#4682 = ORIENTED_EDGE ( 'NONE', *, *, #1487, .F. ) ;
#4683 = EDGE_CURVE ( 'NONE', #2411, #328, #2139, .T. ) ;
#4684 = CARTESIAN_POINT ( 'NONE',  ( -14.67638808697555319, 1.484446970801598990E-11, 38.18288438803429585 ) ) ;
#4685 = ADVANCED_FACE ( 'NONE', ( #4436 ), #3067, .F. ) ;
#4686 = FACE_OUTER_BOUND ( 'NONE', #1036, .T. ) ;
#4687 = CYLINDRICAL_SURFACE ( 'NONE', #3033, 12.50000000000139089 ) ;
#4688 = UNCERTAINTY_MEASURE_WITH_UNIT (LENGTH_MEASURE( 1.000000000000000082E-05 ), #5652, 'distance_accuracy_value', 'NONE');
#4689 = FACE_OUTER_BOUND ( 'NONE', #1391, .T. ) ;
#4690 = VERTEX_POINT ( 'NONE', #2605 ) ;
#4691 = DIRECTION ( 'NONE',  ( -0.000000000000000000, -0.000000000000000000, -1.000000000000000000 ) ) ;
#4692 = ORIENTED_EDGE ( 'NONE', *, *, #4339, .T. ) ;
#4693 = FACE_OUTER_BOUND ( 'NONE', #2171, .T. ) ;
#4694 = CARTESIAN_POINT ( 'NONE',  ( 0.000000000000000000, 0.000000000000000000, 205.0000000000000568 ) ) ;
#4695 = PLANE ( 'NONE',  #3619 ) ;
#4696 = ORIENTED_EDGE ( 'NONE', *, *, #4520, .T. ) ;
#4697 = DIRECTION ( 'NONE',  ( 1.000000000000000000, 0.000000000000000000, 0.000000000000000000 ) ) ;
#4698 = CARTESIAN_POINT ( 'NONE',  ( -56.07162667343609286, 45.16605674834606532, 45.00000000000000711 ) ) ;
#4699 = ORIENTED_EDGE ( 'NONE', *, *, #4845, .T. ) ;
#4700 = ORIENTED_EDGE ( 'NONE', *, *, #241, .F. ) ;
#4701 = CARTESIAN_POINT ( 'NONE',  ( 6.314393452555577824E-13, -67.50000000000002842, -35.00000000000000000 ) ) ;
#4702 = CARTESIAN_POINT ( 'NONE',  ( 0.4914066504972167682, 14.67601930163248625, 38.18288424882400278 ) ) ;
#4703 = CARTESIAN_POINT ( 'NONE',  ( 11.50000000000000355, 67.50000000000000000, 20.00000000000000000 ) ) ;
#4704 = CARTESIAN_POINT ( 'NONE',  ( -9.999999999999998224, 9.999999999999998224, 23.00000000000000000 ) ) ;
#4705 = EDGE_LOOP ( 'NONE', ( #3281, #5589 ) ) ;
#4706 = CARTESIAN_POINT ( 'NONE',  ( -3.645499761006327333, 11.58282027941459091, 30.69674202529824214 ) ) ;
#4707 = CARTESIAN_POINT ( 'NONE',  ( -9.999999999999998224, 9.999999999999998224, 23.00000000000000000 ) ) ;
#4708 = DIRECTION ( 'NONE',  ( -0.000000000000000000, 0.000000000000000000, 1.000000000000000000 ) ) ;
#4709 = ADVANCED_FACE ( 'NONE', ( #2066 ), #5940, .F. ) ;
#4710 = ADVANCED_FACE ( 'NONE', ( #4494 ), #4309, .F. ) ;
#4711 = VERTEX_POINT ( 'NONE', #1207 ) ;
#4712 = DIRECTION ( 'NONE',  ( 0.000000000000000000, 0.000000000000000000, 1.000000000000000000 ) ) ;
#4713 = CARTESIAN_POINT ( 'NONE',  ( 12.49999999999999822, 67.50000000000000000, 20.00000000000000000 ) ) ;
#4714 = CARTESIAN_POINT ( 'NONE',  ( 14.67638808697554964, -1.485455082520059617E-11, 38.18288438803429585 ) ) ;
#4715 = ADVANCED_FACE ( 'NONE', ( #4977 ), #247, .F. ) ;
#4716 = SHAPE_REPRESENTATION ( 'MAS-319', ( #280, #782, #4333, #3144, #4229, #4740, #3938, #1552, #2948, #4846, #2745, #2848, #3829, #1449, #972, #1168, #2147 ), #2351 ) ;
#4717 = VECTOR ( 'NONE', #4104, 1000.000000000000000 ) ;
#4718 =( REPRESENTATION_RELATIONSHIP ('NONE','NONE', #4716, #82 ) REPRESENTATION_RELATIONSHIP_WITH_TRANSFORMATION ( #4424 )SHAPE_REPRESENTATION_RELATIONSHIP( ) );
#4719 = AXIS2_PLACEMENT_3D ( 'NONE', #1855, #5697, #2862 ) ;
#4720 = CARTESIAN_POINT ( 'NONE',  ( 8.975362584346067152, 9.157688896001733525, 22.85246612729342885 ) ) ;
#4721 = ORIENTED_EDGE ( 'NONE', *, *, #3355, .T. ) ;
#4722 = CARTESIAN_POINT ( 'NONE',  ( 52.58482424179591419, -72.37680137756305498, 40.00000000000000000 ) ) ;
#4723 = VECTOR ( 'NONE', #1236, 1000.000000000000000 ) ;
#4724 = ORIENTED_EDGE ( 'NONE', *, *, #3668, .F. ) ;
#4725 = CARTESIAN_POINT ( 'NONE',  ( 0.000000000000000000, 0.000000000000000000, 35.00000000000000000 ) ) ;
#4726 = AXIS2_PLACEMENT_3D ( 'NONE', #5328, #1110, #3481 ) ;
#4727 = EDGE_CURVE ( 'NONE', #5424, #3675, #5442, .T. ) ;
#4728 = DIRECTION ( 'NONE',  ( -0.000000000000000000, -0.000000000000000000, -1.000000000000000000 ) ) ;
#4729 = CARTESIAN_POINT ( 'NONE',  ( 80.08403291566574467, -27.64547812922912939, 40.00000000000000000 ) ) ;
#4730 = ORIENTED_EDGE ( 'NONE', *, *, #1149, .T. ) ;
#4731 = LINE ( 'NONE', #108, #2263 ) ;
#4732 = AXIS2_PLACEMENT_3D ( 'NONE', #3469, #1506, #4400 ) ;
#4733 = CARTESIAN_POINT ( 'NONE',  ( 4.807938790076513591, -13.07368784376655491, 35.76776929191790089 ) ) ;
#4734 = VERTEX_POINT ( 'NONE', #5908 ) ;
#4735 = ORIENTED_EDGE ( 'NONE', *, *, #3794, .T. ) ;
#4736 = CYLINDRICAL_SURFACE ( 'NONE', #3260, 55.00000000000002132 ) ;
#4737 = CARTESIAN_POINT ( 'NONE',  ( -11.33314185116958051, 72.77350886804100583, -35.00000000000000000 ) ) ;
#4738 = PRODUCT ( 'Roll rack Rotating wheel', 'Roll rack Rotating wheel', '', ( #4009 ) ) ;
#4739 = LINE ( 'NONE', #492, #2357 ) ;
#4741 = DIRECTION ( 'NONE',  ( 0.000000000000000000, 0.000000000000000000, 1.000000000000000000 ) ) ;
#4740 = AXIS2_PLACEMENT_3D ( 'NONE', #4268, #1526, #1023 ) ;
#4742 = LINE ( 'NONE', #2874, #5873 ) ;
#4743 = VECTOR ( 'NONE', #2316, 1000.000000000000000 ) ;
#4744 = CARTESIAN_POINT ( 'NONE',  ( 9.793760812180217101, -8.539139919159236314, 27.99841606626185353 ) ) ;
#4745 = EDGE_LOOP ( 'NONE', ( #3883, #2584, #5658, #3371 ) ) ;
#4746 = AXIS2_PLACEMENT_3D ( 'NONE', #3120, #5029, #2538 ) ;
#4747 = CARTESIAN_POINT ( 'NONE',  ( 5.070403286795210678E-14, 8.965668681055127820, 23.09216300389308785 ) ) ;
#4748 = CARTESIAN_POINT ( 'NONE',  ( -4.147343260682110788, 9.916251082295017838, 22.73823205004162418 ) ) ;
#4749 = CARTESIAN_POINT ( 'NONE',  ( 56.72666074499640843, -46.14586675604078891, 35.04915833130704073 ) ) ;
#4750 = ORIENTED_EDGE ( 'NONE', *, *, #2200, .F. ) ;
#4751 = DIRECTION ( 'NONE',  ( 1.000000000000000000, 0.000000000000000000, 0.000000000000000000 ) ) ;
#4752 = VECTOR ( 'NONE', #386, 1000.000000000000114 ) ;
#4753 = EDGE_CURVE ( 'NONE', #720, #4200, #5410, .T. ) ;
#4754 = CARTESIAN_POINT ( 'NONE',  ( -10.99573437649350005, -9.772747244158498603, 38.14042781937033766 ) ) ;
#4755 = AXIS2_PLACEMENT_3D ( 'NONE', #5051, #4038, #2205 ) ;
#4756 = FACE_OUTER_BOUND ( 'NONE', #4237, .T. ) ;
#4757 = AXIS2_PLACEMENT_3D ( 'NONE', #3228, #3174, #2704 ) ;
#4758 = CIRCLE ( 'NONE', #4964, 12.50000000000138911 ) ;
#4759 = EDGE_CURVE ( 'NONE', #6134, #2322, #3220, .T. ) ;
#4760 = CARTESIAN_POINT ( 'NONE',  ( 9.000000000000005329, -8.999999999988066435, 23.06137295785747554 ) ) ;
#4761 = CARTESIAN_POINT ( 'NONE',  ( 14.67638808697554964, 1.797339169375895343E-15, 205.0000000000000568 ) ) ;
#4762 = CIRCLE ( 'NONE', #5068, 80.00000000000000000 ) ;
#4763 = ORIENTED_EDGE ( 'NONE', *, *, #4794, .F. ) ;
#4764 = CARTESIAN_POINT ( 'NONE',  ( 52.58482424179591419, -72.37680137756305498, -79.99999999999998579 ) ) ;
#4765 = DIRECTION ( 'NONE',  ( -0.07194996680737229811, 0.07194996680737240913, 0.9948097328398211037 ) ) ;
#4766 = DIRECTION ( 'NONE',  ( 1.000000000000000000, 0.000000000000000000, 0.000000000000000000 ) ) ;
#4767 = EDGE_LOOP ( 'NONE', ( #3712, #3227, #2344, #3796 ) ) ;
#4768 = CARTESIAN_POINT ( 'NONE',  ( 14.67638808697554964, -1.485455082520059617E-11, 38.18288438803429585 ) ) ;
#4769 = AXIS2_PLACEMENT_3D ( 'NONE', #2016, #1551, #5830 ) ;
#4770 = ADVANCED_FACE ( 'NONE', ( #3097 ), #4818, .F. ) ;
#4771 = CARTESIAN_POINT ( 'NONE',  ( 6.248091806769201284, -11.02058084744346367, 30.63788045528724169 ) ) ;
#4772 = ORIENTED_EDGE ( 'NONE', *, *, #3013, .F. ) ;
#4773 = VERTEX_POINT ( 'NONE', #3031 ) ;
#4774 = PLANE ( 'NONE',  #3558 ) ;
#4775 = FACE_BOUND ( 'NONE', #910, .T. ) ;
#4776 = CARTESIAN_POINT ( 'NONE',  ( -15.00000000000000178, 52.91502622129182498, 20.00000000000000000 ) ) ;
#4777 = CARTESIAN_POINT ( 'NONE',  ( 0.000000000000000000, 0.000000000000000000, 0.000000000000000000 ) ) ;
#4778 = CARTESIAN_POINT ( 'NONE',  ( 10.37777353962571425, 10.37777353962603044, 38.05103295300744293 ) ) ;
#4779 = CARTESIAN_POINT ( 'NONE',  ( 10.23348454756165715, -8.662453428863083005, 30.54531259719474079 ) ) ;
#4780 = ORIENTED_EDGE ( 'NONE', *, *, #4992, .F. ) ;
#4781 = CARTESIAN_POINT ( 'NONE',  ( 6.248212340465907566, 11.02055295301484428, 30.63787875916901626 ) ) ;
#4782 = CARTESIAN_POINT ( 'NONE',  ( 0.8289898103094419657, 9.900940235153615987, 22.73823205004162418 ) ) ;
#4783 = DIRECTION ( 'NONE',  ( 0.000000000000000000, 0.000000000000000000, 1.000000000000000000 ) ) ;
#4784 = VERTEX_POINT ( 'NONE', #748 ) ;
#4785 = CARTESIAN_POINT ( 'NONE',  ( 55.71784976887403928, 21.55374571496248137, 35.00000000000000000 ) ) ;
#4786 = DIRECTION ( 'NONE',  ( -0.000000000000000000, -0.000000000000000000, -1.000000000000000000 ) ) ;
#4787 = CYLINDRICAL_SURFACE ( 'NONE', #2729, 12.49999999999999822 ) ;
#4788 = DIRECTION ( 'NONE',  ( -0.000000000000000000, -0.000000000000000000, 1.000000000000000000 ) ) ;
#4789 = CARTESIAN_POINT ( 'NONE',  ( 7.333173243373136252, -12.74975250248365199, 38.12600698484704509 ) ) ;
#4790 = VERTEX_POINT ( 'NONE', #279 ) ;
#4791 = DIRECTION ( 'NONE',  ( 0.000000000000000000, 0.000000000000000000, 1.000000000000000000 ) ) ;
#4792 = DIRECTION ( 'NONE',  ( -1.000000000000000000, 0.000000000000000000, 0.000000000000000000 ) ) ;
#4793 = EDGE_CURVE ( 'NONE', #1202, #5854, #5320, .T. ) ;
#4794 = EDGE_CURVE ( 'NONE', #1834, #1820, #2094, .T. ) ;
#4795 = CARTESIAN_POINT ( 'NONE',  ( 0.000000000000000000, 0.000000000000000000, -40.00000000000000000 ) ) ;
#4796 = VERTEX_POINT ( 'NONE', #1686 ) ;
#4797 = CARTESIAN_POINT ( 'NONE',  ( 12.46477214039048853, -7.762281575598469985, 38.11692635423789710 ) ) ;
#4798 = CARTESIAN_POINT ( 'NONE',  ( 9.419333092093003401, -9.933255351449997050, 30.50691708577705796 ) ) ;
#4799 = EDGE_LOOP ( 'NONE', ( #24, #4847 ) ) ;
#4800 = ORIENTED_EDGE ( 'NONE', *, *, #5347, .F. ) ;
#4801 = DIRECTION ( 'NONE',  ( 0.000000000000000000, 0.000000000000000000, 1.000000000000000000 ) ) ;
#4802 = FACE_OUTER_BOUND ( 'NONE', #4655, .T. ) ;
#4803 = LINE ( 'NONE', #3333, #1563 ) ;
#4804 = DIRECTION ( 'NONE',  ( 1.000000000000000000, 0.000000000000000000, 0.000000000000000000 ) ) ;
#4805 = EDGE_CURVE ( 'NONE', #4299, #3865, #5504, .T. ) ;
#4806 = CARTESIAN_POINT ( 'NONE',  ( -10.00000000000000178, 10.00000000000000178, 20.00000000000000000 ) ) ;
#4807 = CARTESIAN_POINT ( 'NONE',  ( -7.182140071210238271E-14, 8.916303653273167033E-14, 35.00000000000000000 ) ) ;
#4808 = ORIENTED_EDGE ( 'NONE', *, *, #90, .F. ) ;
#4809 = EDGE_LOOP ( 'NONE', ( #499, #2802, #712, #2640 ) ) ;
#4810 = CARTESIAN_POINT ( 'NONE',  ( -0.9505942623811894920, 12.81596724893641692, 33.26667497053200151 ) ) ;
#4811 = CARTESIAN_POINT ( 'NONE',  ( 9.696021465980070531, 12.35760627049922178, 38.00000000000000000 ) ) ;
#4812 = CARTESIAN_POINT ( 'NONE',  ( 0.000000000000000000, 67.50000000000000000, -19.00000000000000711 ) ) ;
#4813 =( REPRESENTATION_RELATIONSHIP ('NONE','NONE', #4716, #4081 ) REPRESENTATION_RELATIONSHIP_WITH_TRANSFORMATION ( #5899 )SHAPE_REPRESENTATION_RELATIONSHIP( ) );
#4814 = ORIENTED_EDGE ( 'NONE', *, *, #4920, .T. ) ;
#4815 = PLANE ( 'NONE',  #373 ) ;
#4816 = CARTESIAN_POINT ( 'NONE',  ( -12.41454131244164216, -6.563632016262936908, 35.72510948639917672 ) ) ;
#4817 = CARTESIAN_POINT ( 'NONE',  ( -8.309552794738978676, -9.958856949317492990, 22.73823205004162773 ) ) ;
#4818 = CONICAL_SURFACE ( 'NONE', #1161, 80.99999999999998579, 0.7853981633974482790 ) ;
#4819 = DIRECTION ( 'NONE',  ( 1.000000000000000000, 0.000000000000000000, 0.000000000000000000 ) ) ;
#4820 = CARTESIAN_POINT ( 'NONE',  ( 56.72666074499684896, 46.14586675604289212, 35.04915833130718994 ) ) ;
#4821 = VERTEX_POINT ( 'NONE', #3126 ) ;
#4822 = CARTESIAN_POINT ( 'NONE',  ( 0.000000000000000000, 0.000000000000000000, 38.99999999999995737 ) ) ;
#4823 = LINE ( 'NONE', #1853, #1757 ) ;
#4824 = AXIS2_PLACEMENT_3D ( 'NONE', #2671, #1184, #3076 ) ;
#4825 = AXIS2_PLACEMENT_3D ( 'NONE', #238, #3055, #4996 ) ;
#4826 = DIRECTION ( 'NONE',  ( -0.000000000000000000, -0.000000000000000000, -1.000000000000000000 ) ) ;
#4827 = CARTESIAN_POINT ( 'NONE',  ( -9.192833548570215285, -59.02994620157096506, 35.00000000000000000 ) ) ;
#4828 = PRODUCT_DEFINITION_SHAPE ( 'NONE', 'NONE',  #6144 ) ;
#4829 = CARTESIAN_POINT ( 'NONE',  ( 9.772747244158500379, -10.99573437649350005, 38.14042781937034476 ) ) ;
#4830 = AXIS2_PLACEMENT_3D ( 'NONE', #30, #3804, #2790 ) ;
#4831 = AXIS2_PLACEMENT_3D ( 'NONE', #2486, #3376, #2446 ) ;
#4832 = ADVANCED_FACE ( 'NONE', ( #4529 ), #1298, .F. ) ;
#4833 = ORIENTED_EDGE ( 'NONE', *, *, #4091, .T. ) ;
#4834 = CARTESIAN_POINT ( 'NONE',  ( 90.08403291566594362, 27.64547812922851833, -40.00000000000000000 ) ) ;
#4835 = VERTEX_POINT ( 'NONE', #2572 ) ;
#4836 = DIRECTION ( 'NONE',  ( -0.000000000000000000, 0.000000000000000000, 1.000000000000000000 ) ) ;
#4837 = FACE_OUTER_BOUND ( 'NONE', #2006, .T. ) ;
#4838 = DIRECTION ( 'NONE',  ( -1.000000000000000000, -3.054953352033290571E-17, -1.601308366186853033E-17 ) ) ;
#4839 = AXIS2_PLACEMENT_3D ( 'NONE', #1652, #4432, #2063 ) ;
#4840 = DIRECTION ( 'NONE',  ( 0.000000000000000000, -0.000000000000000000, -1.000000000000000000 ) ) ;
#4841 = VECTOR ( 'NONE', #693, 1000.000000000000000 ) ;
#4842 = CARTESIAN_POINT ( 'NONE',  ( 10.27564057804868725, -9.515772848102859172, 33.05475024408053031 ) ) ;
#4843 = ORIENTED_EDGE ( 'NONE', *, *, #154, .T. ) ;
#4844 = EDGE_CURVE ( 'NONE', #2998, #5851, #3025, .T. ) ;
#4845 = EDGE_CURVE ( 'NONE', #149, #4796, #1229, .T. ) ;
#4846 = AXIS2_PLACEMENT_3D ( 'NONE', #5705, #3823, #3426 ) ;
#4847 = ORIENTED_EDGE ( 'NONE', *, *, #5897, .T. ) ;
#4848 = CARTESIAN_POINT ( 'NONE',  ( 1.660914622755446324, 8.965240787521256749, 23.08598164463087343 ) ) ;
#4849 = CARTESIAN_POINT ( 'NONE',  ( 4.166666666666706931, 9.999999999999998224, 23.00000000000000000 ) ) ;
#4850 = CARTESIAN_POINT ( 'NONE',  ( 0.000000000000000000, 0.000000000000000000, -40.00000000000000000 ) ) ;
#4851 = AXIS2_PLACEMENT_3D ( 'NONE', #5422, #4036, #762 ) ;
#4852 = ORIENTED_EDGE ( 'NONE', *, *, #4677, .T. ) ;
#4853 = DIRECTION ( 'NONE',  ( 0.000000000000000000, -0.000000000000000000, 1.000000000000000000 ) ) ;
#4854 = B_SPLINE_CURVE_WITH_KNOTS ( 'NONE', 3,
 ( #2908, #2483, #4371, #5255, #1904, #3799, #5713, #122, #3928, #1971, #1934, #2002, #1568, #1477 ),
 .UNSPECIFIED., .F., .F.,
 ( 4, 2, 2, 2, 2, 2, 4 ),
 ( 0.01144098757322556392, 0.01429571064770015186, 0.01572307218493744496, 0.01715043372217473980, 0.02000515679664932600, 0.02143251833388662084, 0.02285987987112391567 ),
 .UNSPECIFIED. ) ;
#4855 = VECTOR ( 'NONE', #1411, 1000.000000000000000 ) ;
#4856 = ADVANCED_FACE ( 'NONE', ( #4462 ), #5935, .F. ) ;
#4857 = CARTESIAN_POINT ( 'NONE',  ( -10.89081796499577059, 3.137335681707220393E-14, 28.17941898721253580 ) ) ;
#4858 = VERTEX_POINT ( 'NONE', #1650 ) ;
#4859 = CARTESIAN_POINT ( 'NONE',  ( -1.082228759108218918, -15.67638808697554786, 38.00000000000000711 ) ) ;
#4860 = VECTOR ( 'NONE', #5465, 1000.000000000000000 ) ;
#4861 = FACE_OUTER_BOUND ( 'NONE', #224, .T. ) ;
#4862 = CIRCLE ( 'NONE', #4955, 14.67638808697554964 ) ;
#4863 = CARTESIAN_POINT ( 'NONE',  ( 10.37777353962609972, -10.37777353962564852, 38.05103295300747845 ) ) ;
#4864 = EDGE_LOOP ( 'NONE', ( #2768, #4937, #4507, #5889, #5217, #5387, #2457, #4277 ) ) ;
#4865 = CARTESIAN_POINT ( 'NONE',  ( 85.08403291566592941, 27.64547812922851833, 40.00000000000000000 ) ) ;
#4866 = DIRECTION ( 'NONE',  ( -0.000000000000000000, -0.000000000000000000, 1.000000000000000000 ) ) ;
#4867 = AXIS2_PLACEMENT_3D ( 'NONE', #101, #5724, #575 ) ;
#4868 = AXIS2_PLACEMENT_3D ( 'NONE', #5027, #772, #4551 ) ;
#4869 = CARTESIAN_POINT ( 'NONE',  ( 8.999999999999996447, -6.000548030722295145, 23.13502304888910643 ) ) ;
#4870 = ORIENTED_EDGE ( 'NONE', *, *, #3752, .T. ) ;
#4871 = AXIS2_PLACEMENT_3D ( 'NONE', #5901, #4396, #2967 ) ;
#4872 = CARTESIAN_POINT ( 'NONE',  ( 5.390571672161841299, -11.22195964661421819, 30.65936073406735574 ) ) ;
#4873 = ORIENTED_EDGE ( 'NONE', *, *, #3003, .T. ) ;
#4874 = CARTESIAN_POINT ( 'NONE',  ( -68.69027832783800136, -26.57196568621473531, -35.00000000000000000 ) ) ;
#4875 = ORIENTED_EDGE ( 'NONE', *, *, #5522, .T. ) ;
#4876 = CARTESIAN_POINT ( 'NONE',  ( -85.08403291566612836, -27.64547812922793923, -40.00000000000000000 ) ) ;
#4877 = CARTESIAN_POINT ( 'NONE',  ( 11.50000000000000355, 67.50000000000000000, 20.00000000000000000 ) ) ;
#4878 = DIRECTION ( 'NONE',  ( 1.601308366186853341E-17, -5.551115123125781470E-17, -1.000000000000000000 ) ) ;
#4879 = VECTOR ( 'NONE', #143, 1000.000000000000114 ) ;
#4880 = DIRECTION ( 'NONE',  ( 1.000000000000000000, 0.000000000000000000, 0.000000000000000000 ) ) ;
#4881 = DIRECTION ( 'NONE',  ( 1.000000000000000000, 0.000000000000000000, 0.000000000000000000 ) ) ;
#4882 = ORIENTED_EDGE ( 'NONE', *, *, #3493, .T. ) ;
#4883 = ORIENTED_EDGE ( 'NONE', *, *, #5617, .F. ) ;
#4884 = CARTESIAN_POINT ( 'NONE',  ( 4.986905650496099796, 8.963498645742985715, 23.01829711214647745 ) ) ;
#4885 = CARTESIAN_POINT ( 'NONE',  ( 1.657983872361911803, 9.902916272933978803, 22.73823205004162418 ) ) ;
#4886 = DIRECTION ( 'NONE',  ( 0.000000000000000000, 0.000000000000000000, 1.000000000000000000 ) ) ;
#4887 = EDGE_CURVE ( 'NONE', #5727, #3324, #2601, .T. ) ;
#4888 = ORIENTED_EDGE ( 'NONE', *, *, #5533, .T. ) ;
#4889 = FACE_OUTER_BOUND ( 'NONE', #228, .T. ) ;
#4890 = CARTESIAN_POINT ( 'NONE',  ( -11.98089146579572706, -5.533593864557662556, 33.20390238845318009 ) ) ;
#4891 = ORIENTED_EDGE ( 'NONE', *, *, #895, .T. ) ;
#4892 = CARTESIAN_POINT ( 'NONE',  ( 4.147343260682110788, -9.916251082295019614, 22.73823205004162773 ) ) ;
#4893 = EDGE_CURVE ( 'NONE', #4063, #1861, #773, .T. ) ;
#4894 = CARTESIAN_POINT ( 'NONE',  ( 11.42333844578497271, 4.533051537554481314, 30.68084101284746623 ) ) ;
#4895 = CARTESIAN_POINT ( 'NONE',  ( 47.58482424179642578, 72.37680137756268550, -79.99999999999998579 ) ) ;
#4896 = EDGE_LOOP ( 'NONE', ( #5476, #4391, #4147, #4411 ) ) ;
#4897 = LINE ( 'NONE', #3975, #3936 ) ;
#4898 = LINE ( 'NONE', #1078, #5662 ) ;
#4899 = CARTESIAN_POINT ( 'NONE',  ( -2.923529524533197588, -13.51119013911331024, 35.79437308157104525 ) ) ;
#4900 = VERTEX_POINT ( 'NONE', #2188 ) ;
#4901 = CARTESIAN_POINT ( 'NONE',  ( -10.38144361273100280, 10.38144361273100991, 38.10175261887127363 ) ) ;
#4902 = ORIENTED_EDGE ( 'NONE', *, *, #4916, .F. ) ;
#4903 = CARTESIAN_POINT ( 'NONE',  ( 14.18603054855849699, 3.792815487221774973, 38.16899780669729836 ) ) ;
#4904 = CARTESIAN_POINT ( 'NONE',  ( 2.941541598353386116E-14, -7.604078429494091299E-14, 35.00000000000000000 ) ) ;
#4905 = CARTESIAN_POINT ( 'NONE',  ( 58.45671475544992290, -33.74999999999945999, 35.00000000000000000 ) ) ;
#4906 = CARTESIAN_POINT ( 'NONE',  ( 85.08403291566592941, 27.64547812922851833, -79.99999999999998579 ) ) ;
#4907 = EDGE_LOOP ( 'NONE', ( #2360, #5033 ) ) ;
#4908 = EDGE_CURVE ( 'NONE', #5243, #1713, #3000, .T. ) ;
#4909 = VERTEX_POINT ( 'NONE', #5903 ) ;
#4910 = CARTESIAN_POINT ( 'NONE',  ( 10.08321815271041544, 9.378998278013591872, 27.91486726096250948 ) ) ;
#4911 = CARTESIAN_POINT ( 'NONE',  ( 9.981067540164714202, -9.981067540164714202, 22.73823205004162418 ) ) ;
#4912 = PLANE ( 'NONE',  #4627 ) ;
#4913 = ORIENTED_EDGE ( 'NONE', *, *, #1188, .F. ) ;
#4914 = CARTESIAN_POINT ( 'NONE',  ( -8.963498645742985715, -4.986905650496026965, 23.01829711214648100 ) ) ;
#4915 = ORIENTED_EDGE ( 'NONE', *, *, #4098, .F. ) ;
#4916 = EDGE_CURVE ( 'NONE', #5574, #15, #2326, .T. ) ;
#4917 = EDGE_CURVE ( 'NONE', #5256, #1713, #658, .T. ) ;
#4918 = CARTESIAN_POINT ( 'NONE',  ( 1.657983872361815880, -9.902916272933980579, 22.73823205004162773 ) ) ;
#4919 = CARTESIAN_POINT ( 'NONE',  ( 13.68731696136523190, 1.968147360634808329, 35.80501325620552677 ) ) ;
#4920 = EDGE_CURVE ( 'NONE', #6052, #4952, #4628, .T. ) ;
#4921 = ORIENTED_EDGE ( 'NONE', *, *, #5007, .F. ) ;
#4922 = DIRECTION ( 'NONE',  ( 0.000000000000000000, 0.000000000000000000, 1.000000000000000000 ) ) ;
#4923 = LINE ( 'NONE', #2917, #4021 ) ;
#4924 = FACE_BOUND ( 'NONE', #5673, .T. ) ;
#4925 = CARTESIAN_POINT ( 'NONE',  ( -3.645573174172185738, -11.58281169573756131, 30.69674159737795804 ) ) ;
#4926 = ADVANCED_FACE ( 'NONE', ( #3697 ), #364, .F. ) ;
#4927 = EDGE_LOOP ( 'NONE', ( #4225, #5950 ) ) ;
#4928 = CARTESIAN_POINT ( 'NONE',  ( -10.37777353962637505, 10.37777353962536608, 38.05103295300745003 ) ) ;
#4929 = VECTOR ( 'NONE', #1465, 1000.000000000000000 ) ;
#4930 = ORIENTED_EDGE ( 'NONE', *, *, #3415, .F. ) ;
#4931 = DIRECTION ( 'NONE',  ( 0.000000000000000000, 0.000000000000000000, 1.000000000000000000 ) ) ;
#4932 = DIRECTION ( 'NONE',  ( -0.000000000000000000, -0.000000000000000000, -1.000000000000000000 ) ) ;
#4933 = ITEM_DEFINED_TRANSFORMATION ( 'NONE', 'NONE', #4846,  #73 ) ;
#4934 = DIRECTION ( 'NONE',  ( -0.000000000000000000, -0.000000000000000000, 1.000000000000000000 ) ) ;
#4935 = DIRECTION ( 'NONE',  ( -0.1538769332794418798, 0.9880900209011901358, 0.000000000000000000 ) ) ;
#4936 = AXIS2_PLACEMENT_3D ( 'NONE', #5468, #5429, #2024 ) ;
#4937 = ORIENTED_EDGE ( 'NONE', *, *, #5486, .F. ) ;
#4938 = CARTESIAN_POINT ( 'NONE',  ( 7.392961014695930366, 12.01622299351614487, 35.69843844696170976 ) ) ;
#4939 = PRODUCT_DEFINITION_SHAPE ( 'NONE', 'NONE',  #6152 ) ;
#4940 = CARTESIAN_POINT ( 'NONE',  ( 14.79903580929011930, -5.273949241992681891, 38.00000000000000711 ) ) ;
#4941 = CARTESIAN_POINT ( 'NONE',  ( 0.000000000000000000, 67.50000000000000000, -19.00000000000000000 ) ) ;
#4942 = AXIS2_PLACEMENT_3D ( 'NONE', #4150, #6064, #1785 ) ;
#4943 = VECTOR ( 'NONE', #4658, 1000.000000000000000 ) ;
#4944 = VERTEX_POINT ( 'NONE', #863 ) ;
#4945 = PRODUCT_DEFINITION_FORMATION_WITH_SPECIFIED_SOURCE ( 'ANY', '', #4738, .NOT_KNOWN. ) ;
#4946 = CARTESIAN_POINT ( 'NONE',  ( -13.90079966151757596, -4.954970571217796937, 38.30990426830499729 ) ) ;
#4947 = ORIENTED_EDGE ( 'NONE', *, *, #1625, .T. ) ;
#4948 = CIRCLE ( 'NONE', #4851, 80.00000000000000000 ) ;
#4949 = DIRECTION ( 'NONE',  ( -0.000000000000000000, 0.000000000000000000, 1.000000000000000000 ) ) ;
#4950 = CARTESIAN_POINT ( 'NONE',  ( 10.50531938289192624, 7.869812776064879500, 30.57803900350706172 ) ) ;
#4951 = CARTESIAN_POINT ( 'NONE',  ( -67.15076586955559890, 25.97642475653904270, 45.00000000000000711 ) ) ;
#4952 = VERTEX_POINT ( 'NONE', #921 ) ;
#4953 = DIRECTION ( 'NONE',  ( 1.000000000000000000, 0.000000000000000000, 0.000000000000000000 ) ) ;
#4954 = EDGE_CURVE ( 'NONE', #1931, #2370, #3276, .T. ) ;
#4955 = AXIS2_PLACEMENT_3D ( 'NONE', #4694, #5297, #5730 ) ;
#4956 = CARTESIAN_POINT ( 'NONE',  ( 0.9505942623811837189, -12.81596724893641515, 33.26667497053200151 ) ) ;
#4957 = EDGE_LOOP ( 'NONE', ( #479, #731, #4489, #1349 ) ) ;
#4958 = FACE_OUTER_BOUND ( 'NONE', #4957, .T. ) ;
#4959 = AXIS2_PLACEMENT_3D ( 'NONE', #3722, #6105, #2330 ) ;
#4960 = VERTEX_POINT ( 'NONE', #3210 ) ;
#4961 = CARTESIAN_POINT ( 'NONE',  ( -80.08403291566614257, -27.64547812922793923, -40.00000000000000000 ) ) ;
#4962 = DIRECTION ( 'NONE',  ( -8.673617379884026597E-16, -1.000000000000000000, 0.000000000000000000 ) ) ;
#4963 = APPLICATION_PROTOCOL_DEFINITION ( 'draft international standard', 'automotive_design', 1998, #2895 ) ;
#4964 = AXIS2_PLACEMENT_3D ( 'NONE', #4453, #4991, #3950 ) ;
#4965 = CARTESIAN_POINT ( 'NONE',  ( 57.35713647666955950, -46.20154318182373032, 35.13717928826270054 ) ) ;
#4966 = EDGE_CURVE ( 'NONE', #1606, #915, #4141, .T. ) ;
#4967 = CARTESIAN_POINT ( 'NONE',  ( 8.056095891487838412E-14, -1.254589464284425060E-14, -35.00000000000000000 ) ) ;
#4968 = AXIS2_PLACEMENT_3D ( 'NONE', #3756, #3667, #2210 ) ;
#4969 = ORIENTED_EDGE ( 'NONE', *, *, #6136, .F. ) ;
#4970 = ORIENTED_EDGE ( 'NONE', *, *, #4249, .T. ) ;
#4971 = CARTESIAN_POINT ( 'NONE',  ( 0.000000000000000000, 0.000000000000000000, 35.00000000000000000 ) ) ;
#4972 = AXIS2_PLACEMENT_3D ( 'NONE', #1899, #5707, #3429 ) ;
#4973 = CARTESIAN_POINT ( 'NONE',  ( 9.999999999999998224, 5.833333333333301063, 23.00000000000000000 ) ) ;
#4974 = CARTESIAN_POINT ( 'NONE',  ( -27.50000000000000355, -47.63139720814412215, -35.00000000000000000 ) ) ;
#4975 = SHAPE_REPRESENTATION ( 'Roll rack Rotating wheel', ( #73 ), #5734 ) ;
#4976 = VERTEX_POINT ( 'NONE', #3150 ) ;
#4977 = FACE_OUTER_BOUND ( 'NONE', #1761, .T. ) ;
#4978 = CARTESIAN_POINT ( 'NONE',  ( -14.74111653287705792, 1.016991241531514323, 38.35393095385146012 ) ) ;
#4979 = ORIENTED_EDGE ( 'NONE', *, *, #4954, .T. ) ;
#4980 = DIRECTION ( 'NONE',  ( 1.000000000000000000, 0.000000000000000000, 0.000000000000000000 ) ) ;
#4981 = CARTESIAN_POINT ( 'NONE',  ( 8.964415603276487232, 6.652779355836718977, 22.96342386064221941 ) ) ;
#4982 = CYLINDRICAL_SURFACE ( 'NONE', #3437, 5.000000000000004441 ) ;
#4983 = EDGE_LOOP ( 'NONE', ( #4772, #4389, #5653, #3557 ) ) ;
#4984 = VERTEX_POINT ( 'NONE', #2274 ) ;
#4985 = PLANE ( 'NONE',  #4567 ) ;
#4986 = CARTESIAN_POINT ( 'NONE',  ( 2.654236408786701862, -10.78034266696900190, 28.16346921039841433 ) ) ;
#4987 = B_SPLINE_CURVE_WITH_KNOTS ( 'NONE', 3,
 ( #1524, #5871, #714, #207, #4903, #3424, #3019, #2531, #1641, #3510, #5896, #5337, #1114, #2592 ),
 .UNSPECIFIED., .F., .F.,
 ( 4, 2, 2, 2, 2, 2, 4 ),
 ( 0.01144098757322593515, 0.01429571064770019523, 0.01572307218493732700, 0.01715043372217445877, 0.02000515679664871885, 0.02143251833388584715, 0.02285987987112297892 ),
 .UNSPECIFIED. ) ;
#4988 = VERTEX_POINT ( 'NONE', #5558 ) ;
#4989 = LINE ( 'NONE', #296, #2246 ) ;
#4990 = ORIENTED_EDGE ( 'NONE', *, *, #3455, .F. ) ;
#4991 = DIRECTION ( 'NONE',  ( 0.000000000000000000, 0.000000000000000000, 1.000000000000000000 ) ) ;
#4992 = EDGE_CURVE ( 'NONE', #3466, #37, #4193, .T. ) ;
#4993 = EDGE_CURVE ( 'NONE', #4672, #1816, #4420, .T. ) ;
#4994 = CARTESIAN_POINT ( 'NONE',  ( 0.000000000000000000, 0.000000000000000000, 35.00000000000000000 ) ) ;
#4995 = CONTEXT_DEPENDENT_SHAPE_REPRESENTATION ( #813, #4274 ) ;
#4996 = DIRECTION ( 'NONE',  ( -1.000000000000000000, 0.000000000000000000, 0.000000000000000000 ) ) ;
#4997 = FACE_OUTER_BOUND ( 'NONE', #1091, .T. ) ;
#4998 = ORIENTED_EDGE ( 'NONE', *, *, #4844, .F. ) ;
#4999 = EDGE_CURVE ( 'NONE', #5202, #2841, #4519, .T. ) ;
#5000 = CARTESIAN_POINT ( 'NONE',  ( 9.772747244158502156, 10.99573437649350183, 38.14042781937035187 ) ) ;
#5001 = CARTESIAN_POINT ( 'NONE',  ( 9.958856949317492990, -8.309552794738978676, 22.73823205004162418 ) ) ;
#5002 = DIRECTION ( 'NONE',  ( 0.000000000000000000, 0.000000000000000000, -1.000000000000000000 ) ) ;
#5003 = ORIENTED_EDGE ( 'NONE', *, *, #5221, .F. ) ;
#5004 = CARTESIAN_POINT ( 'NONE',  ( 8.056095891487838412E-14, -1.254589464284425060E-14, 35.00000000000000000 ) ) ;
#5005 = CARTESIAN_POINT ( 'NONE',  ( -9.871311131128940985, 2.570253631893349322, 25.61911440830482789 ) ) ;
#5006 = ORIENTED_EDGE ( 'NONE', *, *, #2851, .F. ) ;
#5007 = EDGE_CURVE ( 'NONE', #2468, #1974, #155, .T. ) ;
#5008 = FACE_BOUND ( 'NONE', #5107, .T. ) ;
#5009 = CARTESIAN_POINT ( 'NONE',  ( 11.02058084744346189, 6.248091806769200396, 30.63788045528724524 ) ) ;
#5010 = DIRECTION ( 'NONE',  ( -1.000000000000000000, 0.000000000000000000, 0.000000000000000000 ) ) ;
#5011 = EDGE_LOOP ( 'NONE', ( #4800, #1536, #5276, #1232 ) ) ;
#5012 = ORIENTED_EDGE ( 'NONE', *, *, #2734, .F. ) ;
#5013 = CARTESIAN_POINT ( 'NONE',  ( 0.000000000000000000, 67.50000000000000000, -35.00000000000000000 ) ) ;
#5014 = CARTESIAN_POINT ( 'NONE',  ( -2.570253631893351098, -9.871311131128953420, 25.61911440830483144 ) ) ;
#5015 = VERTEX_POINT ( 'NONE', #1310 ) ;
#5016 = CARTESIAN_POINT ( 'NONE',  ( -12.31015466235495204, -79.04720167209528370, -35.00000000000000711 ) ) ;
#5017 = ORIENTED_EDGE ( 'NONE', *, *, #3653, .T. ) ;
#5018 = CARTESIAN_POINT ( 'NONE',  ( -46.52501622030417394, 37.47620048660903080, 35.00000000000000000 ) ) ;
#5019 = DIRECTION ( 'NONE',  ( 0.000000000000000000, 0.000000000000000000, -1.000000000000000000 ) ) ;
#5020 = PRODUCT_CONTEXT ( 'NONE', #5973, 'mechanical' ) ;
#5021 = CARTESIAN_POINT ( 'NONE',  ( 0.000000000000000000, -67.50000000000000000, -35.00000000000000000 ) ) ;
#5022 = CARTESIAN_POINT ( 'NONE',  ( -11.73806315776973541, -10.43169748385510509, 37.99999999999999289 ) ) ;
#5023 = ADVANCED_FACE ( 'NONE', ( #452 ), #6054, .F. ) ;
#5024 = EDGE_CURVE ( 'NONE', #688, #720, #1706, .T. ) ;
#5025 = AXIS2_PLACEMENT_3D ( 'NONE', #2910, #5787, #5882 ) ;
#5026 = EDGE_LOOP ( 'NONE', ( #1982, #2249, #3354, #1478, #4323, #2616 ) ) ;
#5027 = CARTESIAN_POINT ( 'NONE',  ( 0.000000000000000000, 0.000000000000000000, 20.00000000000000000 ) ) ;
#5028 = DIRECTION ( 'NONE',  ( 1.000000000000000000, 0.000000000000000000, 0.000000000000000000 ) ) ;
#5029 = DIRECTION ( 'NONE',  ( -0.9880900209011902469, -0.1538769332794418798, 0.000000000000000000 ) ) ;
#5030 = DIRECTION ( 'NONE',  ( -0.4999999999999918954, -0.8660254037844433705, 0.000000000000000000 ) ) ;
#5031 = AXIS2_PLACEMENT_3D ( 'NONE', #2900, #2870, #5279 ) ;
#5032 = AXIS2_PLACEMENT_3D ( 'NONE', #5496, #5110, #4638 ) ;
#5033 = ORIENTED_EDGE ( 'NONE', *, *, #3275, .F. ) ;
#5034 = LINE ( 'NONE', #1598, #4841 ) ;
#5035 = EDGE_CURVE ( 'NONE', #1606, #1194, #859, .T. ) ;
#5036 = CARTESIAN_POINT ( 'NONE',  ( -8.970286671637149212, 8.321939193476739050, 22.89273732682886475 ) ) ;
#5037 = AXIS2_PLACEMENT_3D ( 'NONE', #2099, #1179, #5447 ) ;
#5038 = ORIENTED_EDGE ( 'NONE', *, *, #130, .F. ) ;
#5039 = CARTESIAN_POINT ( 'NONE',  ( -10.19494410001831497, 9.858401829237468661, 33.01259202755186095 ) ) ;
#5040 = DIRECTION ( 'NONE',  ( -0.000000000000000000, -0.000000000000000000, 1.000000000000000000 ) ) ;
#5041 = CIRCLE ( 'NONE', #2642, 12.49999999999999822 ) ;
#5042 = DIRECTION ( 'NONE',  ( 1.000000000000000000, 0.000000000000000000, 0.000000000000000000 ) ) ;
#5043 = ADVANCED_FACE ( 'NONE', ( #5116 ), #1283, .T. ) ;
#5044 = CARTESIAN_POINT ( 'NONE',  ( -80.08403291566554572, 27.64547812922971914, -40.00000000000000000 ) ) ;
#5045 = VERTEX_POINT ( 'NONE', #5149 ) ;
#5046 = MECHANICAL_DESIGN_GEOMETRIC_PRESENTATION_REPRESENTATION (  '', ( #1947 ), #3637 ) ;
#5047 = CARTESIAN_POINT ( 'NONE',  ( -6.095889600840176392, -10.32655419438761868, 28.09296952102860345 ) ) ;
#5048 = ORIENTED_EDGE ( 'NONE', *, *, #2126, .T. ) ;
#5049 = FACE_OUTER_BOUND ( 'NONE', #3215, .T. ) ;
#5050 = ORIENTED_EDGE ( 'NONE', *, *, #2230, .F. ) ;
#5051 = CARTESIAN_POINT ( 'NONE',  ( -85.08403291566612836, -27.64547812922793923, 40.00000000000000000 ) ) ;
#5052 = DIRECTION ( 'NONE',  ( 1.000000000000000000, 0.000000000000000000, 0.000000000000000000 ) ) ;
#5053 = VECTOR ( 'NONE', #1994, 1000.000000000000000 ) ;
#5054 = DIRECTION ( 'NONE',  ( -1.000000000000000000, 0.000000000000000000, 0.000000000000000000 ) ) ;
#5055 = AXIS2_PLACEMENT_3D ( 'NONE', #6109, #6055, #1742 ) ;
#5056 = CARTESIAN_POINT ( 'NONE',  ( -9.900940235153615987, -0.8289898103093424897, 22.73823205004162418 ) ) ;
#5057 = VECTOR ( 'NONE', #1227, 1000.000000000000000 ) ;
#5058 = ORIENTED_EDGE ( 'NONE', *, *, #2567, .T. ) ;
#5059 = FACE_OUTER_BOUND ( 'NONE', #2440, .T. ) ;
#5060 = DIRECTION ( 'NONE',  ( 1.000000000000000000, -8.673617379884026597E-16, 0.000000000000000000 ) ) ;
#5061 = FILL_AREA_STYLE_COLOUR ( '', #4548 ) ;
#5062 = CARTESIAN_POINT ( 'NONE',  ( 0.000000000000000000, 0.000000000000000000, 38.00000000000000000 ) ) ;
#5063 = VECTOR ( 'NONE', #858, 1000.000000000000000 ) ;
#5064 = ORIENTED_EDGE ( 'NONE', *, *, #1129, .F. ) ;
#5065 = CARTESIAN_POINT ( 'NONE',  ( 11.71455171164206988, -6.400535080091636964, 33.18278799730941842 ) ) ;
#5066 = VECTOR ( 'NONE', #6036, 1000.000000000000000 ) ;
#5067 = CARTESIAN_POINT ( 'NONE',  ( -10.50531938289192624, 7.869812776064899928, 30.57803900350706883 ) ) ;
#5068 = AXIS2_PLACEMENT_3D ( 'NONE', #2185, #1703, #3604 ) ;
#5069 = ORIENTED_EDGE ( 'NONE', *, *, #4993, .F. ) ;
#5070 = CARTESIAN_POINT ( 'NONE',  ( -6.400384853991316625, 11.71459457793454817, 33.18278774224378225 ) ) ;
#5071 = LINE ( 'NONE', #225, #4723 ) ;
#5072 = EDGE_CURVE ( 'NONE', #945, #4172, #2686, .T. ) ;
#5073 = EDGE_CURVE ( 'NONE', #2569, #2065, #3642, .T. ) ;
#5074 = DIRECTION ( 'NONE',  ( -0.5000000000000039968, 0.8660254037844363761, 0.000000000000000000 ) ) ;
#5075 = VECTOR ( 'NONE', #5342, 1000.000000000000000 ) ;
#5076 = CARTESIAN_POINT ( 'NONE',  ( 52.58482424179643289, 72.37680137756268550, 40.00000000000000000 ) ) ;
#5077 = DIRECTION ( 'NONE',  ( -0.3607836771741531612, -0.9326495259660493309, 0.000000000000000000 ) ) ;
#5078 = ORIENTED_EDGE ( 'NONE', *, *, #1089, .T. ) ;
#5079 = EDGE_CURVE ( 'NONE', #1368, #3265, #4612, .T. ) ;
#5080 = CARTESIAN_POINT ( 'NONE',  ( -5.954811582427138816, -9.638809502600512502, 25.54535933516314472 ) ) ;
#5081 = EDGE_LOOP ( 'NONE', ( #4487, #2113 ) ) ;
#5082 = LINE ( 'NONE', #4575, #297 ) ;
#5083 = ORIENTED_EDGE ( 'NONE', *, *, #1810, .T. ) ;
#5084 = DIRECTION ( 'NONE',  ( -0.000000000000000000, -0.000000000000000000, -1.000000000000000000 ) ) ;
#5085 = CARTESIAN_POINT ( 'NONE',  ( -58.45671475544962448, -33.75000000000001421, 35.00000000000000000 ) ) ;
#5086 = CARTESIAN_POINT ( 'NONE',  ( -12.00215801354939948, 70.99259259259233090, 35.00000000000000000 ) ) ;
#5087 = DIRECTION ( 'NONE',  ( -8.673617379883998001E-16, -1.000000000000000000, 0.000000000000000000 ) ) ;
#5088 = CARTESIAN_POINT ( 'NONE',  ( 10.00265588554886165, -10.00265588554885099, 33.03935750738956756 ) ) ;
#5089 = ORIENTED_EDGE ( 'NONE', *, *, #5364, .F. ) ;
#5090 = DIRECTION ( 'NONE',  ( 0.1538769332794418798, -0.9880900209011901358, 0.000000000000000000 ) ) ;
#5091 = CARTESIAN_POINT ( 'NONE',  ( 14.99999999999995559, -1.301042606982600272E-14, 20.00000000000000000 ) ) ;
#5092 = DIRECTION ( 'NONE',  ( -0.000000000000000000, 0.000000000000000000, 1.000000000000000000 ) ) ;
#5093 = PRODUCT_DEFINITION ( 'UNKNOWN', '', #3536, #1946 ) ;
#5094 = CARTESIAN_POINT ( 'NONE',  ( 11.79779776130986058, -1.839547822007355782, 30.71783115363462358 ) ) ;
#5095 = CARTESIAN_POINT ( 'NONE',  ( -13.50805179034379044, 5.845970755595364388, 38.28811402100272687 ) ) ;
#5096 = VERTEX_POINT ( 'NONE', #6080 ) ;
#5097 = CARTESIAN_POINT ( 'NONE',  ( -2.742560498089726018, 11.69030472852370650, 30.70728637550628548 ) ) ;
#5098 = LINE ( 'NONE', #1875, #3037 ) ;
#5099 = DIRECTION ( 'NONE',  ( 1.000000000000000000, 0.000000000000000000, 0.000000000000000000 ) ) ;
#5100 = EDGE_CURVE ( 'NONE', #688, #3411, #1800, .T. ) ;
#5101 = CARTESIAN_POINT ( 'NONE',  ( 0.000000000000000000, 0.000000000000000000, 20.00000000000000000 ) ) ;
#5102 = CARTESIAN_POINT ( 'NONE',  ( -14.48620990986885637, 2.403201876585511432, 38.17751351274290528 ) ) ;
#5103 = EDGE_CURVE ( 'NONE', #1672, #1178, #4315, .T. ) ;
#5104 = LINE ( 'NONE', #2726, #2476 ) ;
#5105 = ORIENTED_EDGE ( 'NONE', *, *, #128, .F. ) ;
#5106 = DIRECTION ( 'NONE',  ( -0.7071067811865474617, 0.000000000000000000, -0.7071067811865474617 ) ) ;
#5107 = EDGE_LOOP ( 'NONE', ( #4095, #1890 ) ) ;
#5108 = DIRECTION ( 'NONE',  ( -0.9326495259660420034, -0.3607836771741717574, 0.000000000000000000 ) ) ;
#5109 = DIRECTION ( 'NONE',  ( 0.000000000000000000, 0.000000000000000000, 1.000000000000000000 ) ) ;
#5110 = DIRECTION ( 'NONE',  ( 8.673617379884027583E-15, -1.000000000000000000, 0.000000000000000000 ) ) ;
#5111 = CARTESIAN_POINT ( 'NONE',  ( -15.67638808697554786, -1.082228759108213589, 38.00000000000000711 ) ) ;
#5112 = EDGE_CURVE ( 'NONE', #5727, #2811, #3331, .T. ) ;
#5113 = FACE_OUTER_BOUND ( 'NONE', #2086, .T. ) ;
#5114 = VERTEX_POINT ( 'NONE', #1961 ) ;
#5115 = DIRECTION ( 'NONE',  ( 0.000000000000000000, 0.000000000000000000, 1.000000000000000000 ) ) ;
#5116 = FACE_OUTER_BOUND ( 'NONE', #5710, .T. ) ;
#5117 = LINE ( 'NONE', #6081, #3056 ) ;
#5118 = SHAPE_REPRESENTATION_RELATIONSHIP ( 'NONE' , 'NONE' ,  #5596, #5819 ) ;
#5119 = CARTESIAN_POINT ( 'NONE',  ( 13.50805179034378689, -5.845970755595367052, 38.28811402100272687 ) ) ;
#5120 = AXIS2_PLACEMENT_3D ( 'NONE', #1125, #2660, #5852 ) ;
#5121 = CARTESIAN_POINT ( 'NONE',  ( -8.964415574088988592, 6.652784304366588408, 22.96342341013486887 ) ) ;
#5122 = ORIENTED_EDGE ( 'NONE', *, *, #4300, .F. ) ;
#5123 = CARTESIAN_POINT ( 'NONE',  ( -1.902479615894477005, 12.74240908541723805, 33.26151609189631841 ) ) ;
#5125 = CONICAL_SURFACE ( 'NONE', #3028, 11.50000000000000355, 0.7853981633974509435 ) ;
#5124 = CARTESIAN_POINT ( 'NONE',  ( 0.000000000000000000, 0.000000000000000000, 40.00000000000000000 ) ) ;
#5126 =( GEOMETRIC_REPRESENTATION_CONTEXT ( 3 ) GLOBAL_UNCERTAINTY_ASSIGNED_CONTEXT ( ( #3196 ) ) GLOBAL_UNIT_ASSIGNED_CONTEXT ( ( #3129, #4087, #1076 ) ) REPRESENTATION_CONTEXT ( 'NONE', 'WORKASPACE' ) );
#5127 = DIRECTION ( 'NONE',  ( 0.000000000000000000, 0.000000000000000000, 1.000000000000000000 ) ) ;
#5128 = APPLICATION_CONTEXT ( 'automotive_design' ) ;
#5129 = AXIS2_PLACEMENT_3D ( 'NONE', #1293, #4621, #5099 ) ;
#5130 = LINE ( 'NONE', #2255, #4224 ) ;
#5131 = CARTESIAN_POINT ( 'NONE',  ( -12.71058384521454521, 7.353037798771222100, 38.12486502407010391 ) ) ;
#5132 = CONICAL_SURFACE ( 'NONE', #1072, 12.49999999999999822, 0.7853981633974501664 ) ;
#5133 = AXIS2_PLACEMENT_3D ( 'NONE', #3907, #4922, #5824 ) ;
#5134 = CARTESIAN_POINT ( 'NONE',  ( -8.321939193476740826, -8.970286671637149212, 22.89273732682886831 ) ) ;
#5135 = AXIS2_PLACEMENT_3D ( 'NONE', #5200, #4286, #4792 ) ;
#5136 = ORIENTED_EDGE ( 'NONE', *, *, #5876, .F. ) ;
#5137 = CARTESIAN_POINT ( 'NONE',  ( 52.58482424179643289, 72.37680137756268550, -40.00000000000000000 ) ) ;
#5138 = VERTEX_POINT ( 'NONE', #1403 ) ;
#5139 = LINE ( 'NONE', #3573, #2259 ) ;
#5140 = AXIS2_PLACEMENT_3D ( 'NONE', #589, #2467, #4678 ) ;
#5141 = DIRECTION ( 'NONE',  ( 0.000000000000000000, -0.000000000000000000, 1.000000000000000000 ) ) ;
#5142 = EDGE_CURVE ( 'NONE', #4450, #5737, #3859, .T. ) ;
#5143 = PLANE ( 'NONE',  #5032 ) ;
#5144 = CARTESIAN_POINT ( 'NONE',  ( -9.999999999999998224, -9.166666666666657193, 23.00000000000000000 ) ) ;
#5145 = CLOSED_SHELL ( 'NONE', ( #217, #2278, #5227, #968, #5567, #2688, #2772, #849, #6002, #3154, #4372, #884, #4569, #1297 ) ) ;
#5146 = FACE_OUTER_BOUND ( 'NONE', #5698, .T. ) ;
#5147 = ORIENTED_EDGE ( 'NONE', *, *, #324, .F. ) ;
#5148 = DIRECTION ( 'NONE',  ( -0.000000000000000000, -0.000000000000000000, 1.000000000000000000 ) ) ;
#5149 = CARTESIAN_POINT ( 'NONE',  ( -8.999999999999998224, -8.999999999999998224, -167.0000000000000284 ) ) ;
#5150 = EDGE_CURVE ( 'NONE', #4960, #2272, #3502, .T. ) ;
#5151 = CARTESIAN_POINT ( 'NONE',  ( -8.930195544527062879, 11.65680117706474661, 38.09189898655662887 ) ) ;
#5152 = ADVANCED_FACE ( 'NONE', ( #5677, #4775 ), #18, .T. ) ;
#5153 = CARTESIAN_POINT ( 'NONE',  ( 14.74111653287705614, 1.016991241531505441, 38.35393095385146012 ) ) ;
#5154 = AXIS2_PLACEMENT_3D ( 'NONE', #3881, #913, #3267 ) ;
#5155 = ORIENTED_EDGE ( 'NONE', *, *, #3600, .F. ) ;
#5156 = CARTESIAN_POINT ( 'NONE',  ( -1.776762854451772400, 10.85316926984840791, 28.17414535953233923 ) ) ;
#5157 = VECTOR ( 'NONE', #3595, 1000.000000000000000 ) ;
#5158 = CARTESIAN_POINT ( 'NONE',  ( -9.999999999999998224, 9.999999999999998224, 23.00000000000000000 ) ) ;
#5159 = VECTOR ( 'NONE', #4392, 1000.000000000000000 ) ;
#5160 = ORIENTED_EDGE ( 'NONE', *, *, #4564, .F. ) ;
#5161 = DIRECTION ( 'NONE',  ( 1.000000000000000000, 0.000000000000000000, 0.000000000000000000 ) ) ;
#5162 = VECTOR ( 'NONE', #182, 1000.000000000000000 ) ;
#5163 = CARTESIAN_POINT ( 'NONE',  ( 0.000000000000000000, 0.000000000000000000, -39.00000000000001421 ) ) ;
#5164 = AXIS2_PLACEMENT_3D ( 'NONE', #5929, #1527, #4458 ) ;
#5165 = PRODUCT_RELATED_PRODUCT_CATEGORY ( 'part', '', ( #4125 ) ) ;
#5166 = CARTESIAN_POINT ( 'NONE',  ( -7.392961014695934807, -12.01622299351614487, 35.69843844696170976 ) ) ;
#5167 = ORIENTED_EDGE ( 'NONE', *, *, #1633, .T. ) ;
#5168 = CARTESIAN_POINT ( 'NONE',  ( 52.58482424179591419, -72.37680137756305498, 40.00000000000000000 ) ) ;
#5169 = EDGE_LOOP ( 'NONE', ( #524, #2114, #107, #1030 ) ) ;
#5170 = CARTESIAN_POINT ( 'NONE',  ( 68.32682326288367847, -26.05379589900651638, 35.04915833130718994 ) ) ;
#5171 = DIRECTION ( 'NONE',  ( -0.000000000000000000, -0.000000000000000000, -1.000000000000000000 ) ) ;
#5172 = ORIENTED_EDGE ( 'NONE', *, *, #3529, .T. ) ;
#5173 = DIRECTION ( 'NONE',  ( 0.000000000000000000, 0.000000000000000000, 1.000000000000000000 ) ) ;
#5174 = PRODUCT_DEFINITION_SHAPE ( 'NONE', 'NONE',  #6145 ) ;
#5175 = PLANE ( 'NONE',  #4968 ) ;
#5176 = EDGE_CURVE ( 'NONE', #4467, #5045, #198, .T. ) ;
#5177 = ORIENTED_EDGE ( 'NONE', *, *, #3355, .F. ) ;
#5178 = EDGE_LOOP ( 'NONE', ( #5334, #5273, #1814, #560 ) ) ;
#5179 = DIRECTION ( 'NONE',  ( -1.000000000000000000, 0.000000000000000000, 0.000000000000000000 ) ) ;
#5180 = CARTESIAN_POINT ( 'NONE',  ( 80.00000000000000000, 9.797174393178826052E-15, 40.00000000000000000 ) ) ;
#5181 = DIRECTION ( 'NONE',  ( 0.000000000000000000, 1.000000000000000000, 0.000000000000000000 ) ) ;
#5182 = FACE_OUTER_BOUND ( 'NONE', #5775, .T. ) ;
#5183 = CARTESIAN_POINT ( 'NONE',  ( 12.81596724893641337, -2.042222512990850616E-14, 33.26667497053200151 ) ) ;
#5184 = EDGE_CURVE ( 'NONE', #6052, #2828, #5208, .T. ) ;
#5185 =( NAMED_UNIT ( * ) PLANE_ANGLE_UNIT ( ) SI_UNIT ( $, .RADIAN. ) );
#5186 = ORIENTED_EDGE ( 'NONE', *, *, #1839, .F. ) ;
#5187 = CARTESIAN_POINT ( 'NONE',  ( -4.666802875123988947, 12.24718835365691305, 33.22501703466258505 ) ) ;
#5188 = ORIENTED_EDGE ( 'NONE', *, *, #4683, .T. ) ;
#5189 = CARTESIAN_POINT ( 'NONE',  ( 9.500000000000008882, 67.50000000000000000, 20.00000000000000000 ) ) ;
#5190 = EDGE_LOOP ( 'NONE', ( #724, #4700, #4990, #4259 ) ) ;
#5191 = CARTESIAN_POINT ( 'NONE',  ( 52.58482424179591419, -72.37680137756305498, -40.00000000000000000 ) ) ;
#5192 = EDGE_CURVE ( 'NONE', #3886, #1883, #5528, .T. ) ;
#5193 = CARTESIAN_POINT ( 'NONE',  ( -10.67327843797380815, -8.785602912694960409, 33.09221060678261495 ) ) ;
#5194 = CARTESIAN_POINT ( 'NONE',  ( -12.46477214039063597, 7.762281575598230177, 38.11692635423788289 ) ) ;
#5195 = CARTESIAN_POINT ( 'NONE',  ( -15.00000000000000000, 50.91502622129181788, -20.00000000000000000 ) ) ;
#5196 = ORIENTED_EDGE ( 'NONE', *, *, #5649, .F. ) ;
#5197 = DIRECTION ( 'NONE',  ( 0.6273063437270329779, -0.7787725926866080339, 0.000000000000000000 ) ) ;
#5198 = ORIENTED_EDGE ( 'NONE', *, *, #1511, .F. ) ;
#5199 = CARTESIAN_POINT ( 'NONE',  ( 9.074396217167167933, 58.26942451214404173, 35.00000000000000000 ) ) ;
#5200 = CARTESIAN_POINT ( 'NONE',  ( 0.000000000000000000, 0.000000000000000000, 205.0000000000000568 ) ) ;
#5201 = DIRECTION ( 'NONE',  ( -0.000000000000000000, -0.000000000000000000, -1.000000000000000000 ) ) ;
#5202 = VERTEX_POINT ( 'NONE', #4737 ) ;
#5203 = CARTESIAN_POINT ( 'NONE',  ( 9.192833548570416013, -59.02994620156847105, 35.00000000000000000 ) ) ;
#5204 = CARTESIAN_POINT ( 'NONE',  ( 8.539045536263008884, -9.793778397576030414, 27.99842134739335364 ) ) ;
#5205 = ORIENTED_EDGE ( 'NONE', *, *, #164, .F. ) ;
#5206 = EDGE_LOOP ( 'NONE', ( #5543, #4540, #5048, #1459, #1243, #3771, #2783 ) ) ;
#5207 = DIRECTION ( 'NONE',  ( -0.000000000000000000, 0.000000000000000000, 1.000000000000000000 ) ) ;
#5208 = LINE ( 'NONE', #1021, #2437 ) ;
#5209 = CARTESIAN_POINT ( 'NONE',  ( 9.999999999999998224, 9.999999999999998224, 20.00000000000000000 ) ) ;
#5210 = DIRECTION ( 'NONE',  ( 6.303473954557536582E-18, -1.499031448860895019E-16, -1.000000000000000000 ) ) ;
#5211 = EDGE_CURVE ( 'NONE', #413, #2151, #3395, .T. ) ;
#5212 = CARTESIAN_POINT ( 'NONE',  ( -1.301042606982566193E-13, 14.99999999999956124, 35.00000000000000000 ) ) ;
#5213 = ADVANCED_FACE ( 'NONE', ( #2074 ), #2927, .F. ) ;
#5214 = PLANE ( 'NONE',  #1668 ) ;
#5215 = B_SPLINE_CURVE_WITH_KNOTS ( 'NONE', 3,
 ( #1776, #2275, #2304, #3698, #2715, #4613, #5585, #4194, #5559, #365, #864, #2805, #4702, #453, #2744, #4079, #5994, #2777, #1707, #839, #5526, #5644, #5151, #4142, #3184, #1311 ),
 .UNSPECIFIED., .F., .F.,
 ( 4, 2, 2, 2, 2, 2, 2, 2, 2, 2, 2, 2, 4 ),
 ( 0.000000000000000000, 0.002857484983890443489, 0.004286227475835666101, 0.005714969967780886978, 0.008572454951671333936, 0.01000119744361655655, 0.01142993993556177743, 0.01428742491945222091, 0.01571616741139744353, 0.01714490990334266440, 0.02000239488723310963, 0.02143113737917832703, 0.02285987987112354444 ),
 .UNSPECIFIED. ) ;
#5216 = B_SPLINE_CURVE_WITH_KNOTS ( 'NONE', 3,
 ( #115, #628, #717, #2506, #2057, #2534 ),
 .UNSPECIFIED., .F., .F.,
 ( 4, 2, 4 ),
 ( 2.991083242018516676E-05, 0.007589224902226409351, 0.01514853897203263453 ),
 .UNSPECIFIED. ) ;
#5217 = ORIENTED_EDGE ( 'NONE', *, *, #4993, .T. ) ;
#5218 = CARTESIAN_POINT ( 'NONE',  ( 2.570253631893349766, 9.871311131128940985, 25.61911440830482789 ) ) ;
#5219 = CARTESIAN_POINT ( 'NONE',  ( 9.999999999999998224, 8.333333333333316162, 23.00000000000000000 ) ) ;
#5220 = CYLINDRICAL_SURFACE ( 'NONE', #2737, 4.999999999999990230 ) ;
#5221 = EDGE_CURVE ( 'NONE', #6071, #1883, #1626, .T. ) ;
#5222 = ORIENTED_EDGE ( 'NONE', *, *, #5883, .F. ) ;
#5223 = DIRECTION ( 'NONE',  ( -1.000000000000000000, 0.000000000000000000, 0.000000000000000000 ) ) ;
#5224 = FACE_OUTER_BOUND ( 'NONE', #4304, .T. ) ;
#5225 = VECTOR ( 'NONE', #289, 1000.000000000000000 ) ;
#5226 = CARTESIAN_POINT ( 'NONE',  ( 9.981067540164714202, -9.981067540164714202, 22.73823205004162773 ) ) ;
#5227 = ADVANCED_FACE ( 'NONE', ( #4802 ), #5125, .T. ) ;
#5228 = VECTOR ( 'NONE', #5201, 1000.000000000000000 ) ;
#5229 = CARTESIAN_POINT ( 'NONE',  ( -10.00265588554884744, 10.00265588554886165, 33.03935750738952493 ) ) ;
#5230 = CARTESIAN_POINT ( 'NONE',  ( -100.0000000000000000, 0.000000000000000000, -39.00000000000002842 ) ) ;
#5231 = AXIS2_PLACEMENT_3D ( 'NONE', #5656, #1380, #1783 ) ;
#5232 = ORIENTED_EDGE ( 'NONE', *, *, #4300, .T. ) ;
#5233 = DIRECTION ( 'NONE',  ( 1.000000000000000000, 0.000000000000000000, 0.000000000000000000 ) ) ;
#5234 = AXIS2_PLACEMENT_3D ( 'NONE', #465, #2695, #5161 ) ;
#5235 = CARTESIAN_POINT ( 'NONE',  ( -14.99999999999995559, -1.301042606982600272E-14, 20.00000000000000000 ) ) ;
#5236 = VECTOR ( 'NONE', #4568, 1000.000000000000114 ) ;
#5237 = DIRECTION ( 'NONE',  ( 1.000000000000000000, 0.000000000000000000, 0.000000000000000000 ) ) ;
#5238 = EDGE_LOOP ( 'NONE', ( #1891, #2792, #4479, #657 ) ) ;
#5239 = FACE_OUTER_BOUND ( 'NONE', #488, .T. ) ;
#5240 = CARTESIAN_POINT ( 'NONE',  ( 9.618700053625529378, -10.13908112636436520, 30.46372964425718521 ) ) ;
#5241 = CARTESIAN_POINT ( 'NONE',  ( 4.273103006804781501, -9.778265433844634202, 25.59105575288734968 ) ) ;
#5242 = CIRCLE ( 'NONE', #4537, 9.500000000000005329 ) ;
#5243 = VERTEX_POINT ( 'NONE', #592 ) ;
#5244 = ORIENTED_EDGE ( 'NONE', *, *, #4466, .T. ) ;
#5245 = DIRECTION ( 'NONE',  ( -0.000000000000000000, -0.000000000000000000, -1.000000000000000000 ) ) ;
#5246 = DIRECTION ( 'NONE',  ( 0.7787725926866163606, -0.6273063437270225418, 0.000000000000000000 ) ) ;
#5247 = DIRECTION ( 'NONE',  ( -0.000000000000000000, -0.000000000000000000, -1.000000000000000000 ) ) ;
#5248 = DIRECTION ( 'NONE',  ( 1.566902880027386494E-17, -5.324870654159525494E-17, -0.9999999999999998890 ) ) ;
#5249 = CYLINDRICAL_SURFACE ( 'NONE', #4661, 80.00000000000000000 ) ;
#5250 = FACE_OUTER_BOUND ( 'NONE', #3110, .T. ) ;
#5251 = ORIENTED_EDGE ( 'NONE', *, *, #3679, .F. ) ;
#5252 = CIRCLE ( 'NONE', #5946, 12.50000000000000000 ) ;
#5253 = CARTESIAN_POINT ( 'NONE',  ( 3.322922547535530846, 8.964120815521452457, 23.06129036953744915 ) ) ;
#5254 = CARTESIAN_POINT ( 'NONE',  ( 5.273949241992681891, 14.79903580929012108, 38.00000000000000711 ) ) ;
#5255 = CARTESIAN_POINT ( 'NONE',  ( -14.30354638250589794, -3.321916882804577753, 38.17191617598168563 ) ) ;
#5256 = VERTEX_POINT ( 'NONE', #4325 ) ;
#5257 = DIRECTION ( 'NONE',  ( 0.1538769332794358846, 0.9880900209011910240, 0.000000000000000000 ) ) ;
#5258 = AXIS2_PLACEMENT_3D ( 'NONE', #2302, #3149, #2273 ) ;
#5259 = CARTESIAN_POINT ( 'NONE',  ( -8.975362584346067152, -9.157688896001735301, 22.85246612729342885 ) ) ;
#5260 = EDGE_CURVE ( 'NONE', #4200, #1345, #2336, .T. ) ;
#5261 = EDGE_CURVE ( 'NONE', #3300, #4909, #1431, .T. ) ;
#5262 = CARTESIAN_POINT ( 'NONE',  ( -9.144590365090035533, -9.969668718019493170, 22.73823205004162773 ) ) ;
#5263 = CIRCLE ( 'NONE', #889, 5.000000000000004441 ) ;
#5264 = VECTOR ( 'NONE', #4543, 1000.000000000000000 ) ;
#5265 = DIRECTION ( 'NONE',  ( -0.000000000000000000, -0.000000000000000000, -1.000000000000000000 ) ) ;
#5266 = EDGE_CURVE ( 'NONE', #2727, #5910, #462, .T. ) ;
#5267 = DIRECTION ( 'NONE',  ( 0.000000000000000000, -0.000000000000000000, -1.000000000000000000 ) ) ;
#5268 = VECTOR ( 'NONE', #3719, 999.9999999999998863 ) ;
#5269 = ORIENTED_EDGE ( 'NONE', *, *, #248, .T. ) ;
#5270 = CARTESIAN_POINT ( 'NONE',  ( 67.92475106770454829, -25.56373185532678960, 35.00000000000000000 ) ) ;
#5271 = DIRECTION ( 'NONE',  ( 1.000000000000000000, 0.000000000000000000, 0.000000000000000000 ) ) ;
#5272 = CARTESIAN_POINT ( 'NONE',  ( 9.999999999999998224, 9.999999999999998224, 23.00000000000000000 ) ) ;
#5273 = ORIENTED_EDGE ( 'NONE', *, *, #5073, .T. ) ;
#5274 = DIRECTION ( 'NONE',  ( -0.000000000000000000, -0.000000000000000000, -1.000000000000000000 ) ) ;
#5275 = CARTESIAN_POINT ( 'NONE',  ( 9.994658916190591214, -8.983694681928700021, 22.80938439471026058 ) ) ;
#5276 = ORIENTED_EDGE ( 'NONE', *, *, #1846, .T. ) ;
#5277 = VERTEX_POINT ( 'NONE', #527 ) ;
#5278 = CARTESIAN_POINT ( 'NONE',  ( 15.00000000000000178, 52.91502622129182498, -20.00000000000000000 ) ) ;
#5279 = DIRECTION ( 'NONE',  ( 1.000000000000000000, 0.000000000000000000, 0.000000000000000000 ) ) ;
#5280 = DIRECTION ( 'NONE',  ( -0.7071067811865489050, 8.659560562354950115E-17, 0.7071067811865462405 ) ) ;
#5281 = DIRECTION ( 'NONE',  ( -0.8160810397761946167, 0.5779374849564660188, 0.000000000000000000 ) ) ;
#5282 = DIRECTION ( 'NONE',  ( -0.000000000000000000, 0.000000000000000000, 1.000000000000000000 ) ) ;
#5283 = FACE_OUTER_BOUND ( 'NONE', #3594, .T. ) ;
#5284 = ORIENTED_EDGE ( 'NONE', *, *, #5261, .F. ) ;
#5285 = CARTESIAN_POINT ( 'NONE',  ( 0.8304760625349936198, 8.965668681055126044, 23.09216300389308074 ) ) ;
#5286 = CARTESIAN_POINT ( 'NONE',  ( 8.069545871843432749, 13.47611570251764768, 37.99999999999999289 ) ) ;
#5287 = DIRECTION ( 'NONE',  ( -0.000000000000000000, -0.000000000000000000, -1.000000000000000000 ) ) ;
#5288 = ORIENTED_EDGE ( 'NONE', *, *, #1913, .F. ) ;
#5289 = DIRECTION ( 'NONE',  ( 0.000000000000000000, -1.000000000000000000, 0.000000000000000000 ) ) ;
#5290 = CARTESIAN_POINT ( 'NONE',  ( -13.11530391917000316, -6.736970939972939831, 38.26632377370044225 ) ) ;
#5291 = CARTESIAN_POINT ( 'NONE',  ( -1.666666666666713814, -9.999999999999998224, 23.00000000000000000 ) ) ;
#5292 = EDGE_CURVE ( 'NONE', #5786, #3029, #5888, .T. ) ;
#5293 = CARTESIAN_POINT ( 'NONE',  ( 80.08403291566592941, 27.64547812922851833, -40.00000000000000000 ) ) ;
#5294 = CARTESIAN_POINT ( 'NONE',  ( 55.48030965892933608, 45.89047003626479437, 35.00000000000000000 ) ) ;
#5295 = ORIENTED_EDGE ( 'NONE', *, *, #3030, .F. ) ;
#5296 = CARTESIAN_POINT ( 'NONE',  ( -12.49999999999999822, 67.50000000000000000, 20.00000000000000000 ) ) ;
#5297 = DIRECTION ( 'NONE',  ( 0.000000000000000000, 0.000000000000000000, 1.000000000000000000 ) ) ;
#5298 = DIRECTION ( 'NONE',  ( 0.7071067811865464625, -0.7071067811865486830, 0.000000000000000000 ) ) ;
#5299 = ORIENTED_EDGE ( 'NONE', *, *, #3350, .T. ) ;
#5300 = ADVANCED_FACE ( 'NONE', ( #5483 ), #4595, .F. ) ;
#5301 = FACE_BOUND ( 'NONE', #4927, .T. ) ;
#5302 = CARTESIAN_POINT ( 'NONE',  ( 6.736970939972923844, -13.11530391917000316, 38.26632377370044935 ) ) ;
#5303 = ORIENTED_EDGE ( 'NONE', *, *, #3247, .F. ) ;
#5304 = ORIENTED_EDGE ( 'NONE', *, *, #320, .T. ) ;
#5305 = CARTESIAN_POINT ( 'NONE',  ( 0.000000000000000000, 0.000000000000000000, 35.00000000000000000 ) ) ;
#5306 = CARTESIAN_POINT ( 'NONE',  ( 5.114554293134526134E-14, 6.349488965209711204E-14, 35.00000000000000000 ) ) ;
#5307 = LINE ( 'NONE', #1896, #4251 ) ;
#5308 = CARTESIAN_POINT ( 'NONE',  ( 0.000000000000000000, 0.000000000000000000, 0.000000000000000000 ) ) ;
#5309 = EDGE_CURVE ( 'NONE', #4004, #1816, #2611, .T. ) ;
#5310 = CARTESIAN_POINT ( 'NONE',  ( 8.983694681928700021, -9.994658916190592990, 22.80938439471025703 ) ) ;
#5311 = ORIENTED_EDGE ( 'NONE', *, *, #2710, .T. ) ;
#5312 = CARTESIAN_POINT ( 'NONE',  ( 1.016991241531516987, 14.74111653287705792, 38.35393095385146012 ) ) ;
#5313 = CARTESIAN_POINT ( 'NONE',  ( 11.08488032081242203, 11.08488032081242203, 38.00000000000000000 ) ) ;
#5314 = DIRECTION ( 'NONE',  ( 0.000000000000000000, 0.000000000000000000, 1.000000000000000000 ) ) ;
#5315 = ORIENTED_EDGE ( 'NONE', *, *, #1680, .T. ) ;
#5316 = DIRECTION ( 'NONE',  ( 0.000000000000000000, 0.000000000000000000, 1.000000000000000000 ) ) ;
#5317 = CARTESIAN_POINT ( 'NONE',  ( -12.74242197681752309, 1.902388932222470963, 33.26151580524048512 ) ) ;
#5318 = VERTEX_POINT ( 'NONE', #4000 ) ;
#5319 = CARTESIAN_POINT ( 'NONE',  ( 0.8333333333332849646, -10.00000000000000000, 23.00000000000000355 ) ) ;
#5320 = CIRCLE ( 'NONE', #2923, 12.49999999999999822 ) ;
#5321 = CARTESIAN_POINT ( 'NONE',  ( -62.30180741492890206, 50.18450749816231848, 35.00000000000000000 ) ) ;
#5322 = DIRECTION ( 'NONE',  ( 0.000000000000000000, 0.000000000000000000, 1.000000000000000000 ) ) ;
#5323 = EDGE_LOOP ( 'NONE', ( #828, #5122, #204, #985 ) ) ;
#5324 = LINE ( 'NONE', #1074, #184 ) ;
#5325 = CARTESIAN_POINT ( 'NONE',  ( 9.500000000000008882, 67.50000000000000000, -20.00000000000000000 ) ) ;
#5326 = AXIS2_PLACEMENT_3D ( 'NONE', #2169, #4062, #4118 ) ;
#5327 = VECTOR ( 'NONE', #2207, 1000.000000000000114 ) ;
#5328 = CARTESIAN_POINT ( 'NONE',  ( 0.000000000000000000, 9.999999999999998224, 20.00000000000000000 ) ) ;
#5329 = ORIENTED_EDGE ( 'NONE', *, *, #1788, .F. ) ;
#5330 = CARTESIAN_POINT ( 'NONE',  ( 0.000000000000000000, 0.000000000000000000, 38.00000000000000000 ) ) ;
#5331 = CARTESIAN_POINT ( 'NONE',  ( 9.322893336083156512, -9.590870124851306855, 27.95908392747358917 ) ) ;
#5332 = CIRCLE ( 'NONE', #1935, 80.00000000000000000 ) ;
#5333 = CIRCLE ( 'NONE', #2135, 80.00000000000000000 ) ;
#5334 = ORIENTED_EDGE ( 'NONE', *, *, #698, .T. ) ;
#5335 =( NAMED_UNIT ( * ) SI_UNIT ( $, .STERADIAN. ) SOLID_ANGLE_UNIT ( ) );
#5336 = ORIENTED_EDGE ( 'NONE', *, *, #5906, .T. ) ;
#5337 = CARTESIAN_POINT ( 'NONE',  ( 11.04414289254854253, 9.677595944628125224, 38.07286884698773832 ) ) ;
#5338 = EDGE_CURVE ( 'NONE', #537, #730, #4501, .T. ) ;
#5339 = DIRECTION ( 'NONE',  ( -0.9326495259660420034, -0.3607836771741717574, 0.000000000000000000 ) ) ;
#5340 =( LENGTH_UNIT ( ) NAMED_UNIT ( * ) SI_UNIT ( .MILLI., .METRE. ) );
#5341 = AXIS2_PLACEMENT_3D ( 'NONE', #2282, #2347, #2252 ) ;
#5342 = DIRECTION ( 'NONE',  ( -0.000000000000000000, -0.000000000000000000, -1.000000000000000000 ) ) ;
#5343 = CARTESIAN_POINT ( 'NONE',  ( 10.99573437649350005, -9.772747244158503932, 38.14042781937035187 ) ) ;
#5344 = CONICAL_SURFACE ( 'NONE', #1943, 100.0000000000000000, 0.7853981633974621568 ) ;
#5345 = VECTOR ( 'NONE', #5839, 1000.000000000000000 ) ;
#5346 = VERTEX_POINT ( 'NONE', #5510 ) ;
#5347 = EDGE_CURVE ( 'NONE', #5498, #1368, #2826, .T. ) ;
#5348 = CARTESIAN_POINT ( 'NONE',  ( 0.9193131588476516347, 11.85339260696609287, 30.72304697887226510 ) ) ;
#5349 = CARTESIAN_POINT ( 'NONE',  ( -57.35713647667095927, -46.20154318182582642, 35.13717928826310555 ) ) ;
#5350 = VECTOR ( 'NONE', #4691, 1000.000000000000000 ) ;
#5351 = ORIENTED_EDGE ( 'NONE', *, *, #1483, .T. ) ;
#5352 = DIRECTION ( 'NONE',  ( -0.000000000000000000, -0.000000000000000000, 1.000000000000000000 ) ) ;
#5353 = CARTESIAN_POINT ( 'NONE',  ( -12.81596724893641337, 0.9505942623812192460, 33.26667497053200151 ) ) ;
#5354 = ORIENTED_EDGE ( 'NONE', *, *, #5826, .T. ) ;
#5355 = FACE_OUTER_BOUND ( 'NONE', #1688, .T. ) ;
#5356 = VECTOR ( 'NONE', #5247, 1000.000000000000000 ) ;
#5357 = CARTESIAN_POINT ( 'NONE',  ( 8.964120776013636771, 3.322926169935025431, 23.06129021161080317 ) ) ;
#5358 = VECTOR ( 'NONE', #894, 1000.000000000000000 ) ;
#5359 = CARTESIAN_POINT ( 'NONE',  ( 0.000000000000000000, 0.000000000000000000, 38.99999999999995737 ) ) ;
#5360 = ORIENTED_EDGE ( 'NONE', *, *, #1669, .T. ) ;
#5361 = CARTESIAN_POINT ( 'NONE',  ( -14.67638808697554964, 0.000000000000000000, 205.0000000000000568 ) ) ;
#5362 = AXIS2_PLACEMENT_3D ( 'NONE', #2493, #4380, #1546 ) ;
#5363 = B_SPLINE_CURVE_WITH_KNOTS ( 'NONE', 3,
 ( #4068, #5985, #735, #1697, #5514, #1242 ),
 .UNSPECIFIED., .F., .F.,
 ( 4, 2, 4 ),
 ( 0.002357188415687244253, 0.01135824717474481077, 0.02035930593380237685 ),
 .UNSPECIFIED. ) ;
#5364 = EDGE_CURVE ( 'NONE', #3660, #4090, #666, .T. ) ;
#5365 = CARTESIAN_POINT ( 'NONE',  ( 50.91502622129181788, 12.00000000000000355, -35.00000000000000000 ) ) ;
#5366 = CARTESIAN_POINT ( 'NONE',  ( -45.92560378283280187, -36.99336990414421678, -35.00000000000000000 ) ) ;
#5367 = AXIS2_PLACEMENT_3D ( 'NONE', #971, #3842, #4819 ) ;
#5368 = CARTESIAN_POINT ( 'NONE',  ( -3.322922547535532178, -8.964120815521452457, 23.06129036953745270 ) ) ;
#5369 = VERTEX_POINT ( 'NONE', #1238 ) ;
#5370 = VERTEX_POINT ( 'NONE', #5044 ) ;
#5371 = DIRECTION ( 'NONE',  ( -0.07194996680737208994, 0.07194996680737265893, -0.9948097328398211037 ) ) ;
#5372 = DIRECTION ( 'NONE',  ( 1.000000000000000000, 0.000000000000000000, 0.000000000000000000 ) ) ;
#5373 = VECTOR ( 'NONE', #1433, 1000.000000000000000 ) ;
#5374 = CYLINDRICAL_SURFACE ( 'NONE', #4364, 12.49999999999999645 ) ;
#5375 = CARTESIAN_POINT ( 'NONE',  ( 46.52501622030442974, -37.47620048660870395, 35.00000000000000000 ) ) ;
#5376 = VERTEX_POINT ( 'NONE', #755 ) ;
#5377 = EDGE_CURVE ( 'NONE', #6119, #3856, #4029, .T. ) ;
#5378 = EDGE_CURVE ( 'NONE', #382, #5383, #255, .T. ) ;
#5379 = ORIENTED_EDGE ( 'NONE', *, *, #1051, .F. ) ;
#5380 = DIRECTION ( 'NONE',  ( 1.000000000000000000, 0.000000000000000000, 0.000000000000000000 ) ) ;
#5381 = CARTESIAN_POINT ( 'NONE',  ( 9.939337621248920840, -6.642184745761470666, 22.73823205004162418 ) ) ;
#5382 = CARTESIAN_POINT ( 'NONE',  ( 57.35713647667095927, 46.20154318182582642, 35.13717928826310555 ) ) ;
#5383 = VERTEX_POINT ( 'NONE', #1665 ) ;
#5384 = CARTESIAN_POINT ( 'NONE',  ( 27.60043906316099083, 27.60043906316109386, 35.00000000000000000 ) ) ;
#5385 = ADVANCED_FACE ( 'NONE', ( #4570 ), #4112, .F. ) ;
#5386 = CARTESIAN_POINT ( 'NONE',  ( -12.74411457810409409, -5.685785403169723473, 35.74643938915853880 ) ) ;
#5387 = ORIENTED_EDGE ( 'NONE', *, *, #5309, .F. ) ;
#5388 = CARTESIAN_POINT ( 'NONE',  ( 4.260267006495011444, -15.12434353048566571, 38.00000000000000711 ) ) ;
#5389 = PRODUCT_DEFINITION_SHAPE ( 'NONE', 'NONE',  #6149 ) ;
#5390 = ADVANCED_FACE ( 'NONE', ( #1692 ), #3593, .F. ) ;
#5391 = EDGE_LOOP ( 'NONE', ( #3399, #3820, #1241, #927 ) ) ;
#5392 = DIRECTION ( 'NONE',  ( 1.000000000000000000, 0.000000000000000000, 0.000000000000000000 ) ) ;
#5393 = DIRECTION ( 'NONE',  ( -0.000000000000000000, -0.000000000000000000, -1.000000000000000000 ) ) ;
#5394 = CARTESIAN_POINT ( 'NONE',  ( -4.532931003857846086, -11.42336634021359387, 30.68084270896568810 ) ) ;
#5395 = VERTEX_POINT ( 'NONE', #3133 ) ;
#5396 = DIRECTION ( 'NONE',  ( 1.000000000000000000, 0.000000000000000000, 0.000000000000000000 ) ) ;
#5397 = EDGE_LOOP ( 'NONE', ( #2466, #2960, #110, #28 ) ) ;
#5398 = CARTESIAN_POINT ( 'NONE',  ( 85.08403291566575888, -27.64547812922912939, 40.00000000000000000 ) ) ;
#5399 = DIRECTION ( 'NONE',  ( 1.000000000000000000, 0.000000000000000000, 0.000000000000000000 ) ) ;
#5400 = CONTEXT_DEPENDENT_SHAPE_REPRESENTATION ( #4718, #1988 ) ;
#5401 = FACE_OUTER_BOUND ( 'NONE', #1429, .T. ) ;
#5402 = CARTESIAN_POINT ( 'NONE',  ( -9.981067540164714202, -9.981067540164714202, 22.73823205004162418 ) ) ;
#5403 = EDGE_LOOP ( 'NONE', ( #5303, #4373, #2934, #1851, #2762, #2031 ) ) ;
#5404 = CARTESIAN_POINT ( 'NONE',  ( 10.38144361273100635, 10.38144361273100458, 38.10175261887127363 ) ) ;
#5405 = CARTESIAN_POINT ( 'NONE',  ( 9.910574073276151807, 3.317157231508560677, 22.73823205004162418 ) ) ;
#5406 =( LENGTH_UNIT ( ) NAMED_UNIT ( * ) SI_UNIT ( .MILLI., .METRE. ) );
#5407 = ADVANCED_FACE ( 'NONE', ( #2130 ), #227, .F. ) ;
#5408 = ADVANCED_FACE ( 'NONE', ( #2198 ), #2699, .T. ) ;
#5409 = ORIENTED_EDGE ( 'NONE', *, *, #2161, .T. ) ;
#5410 = LINE ( 'NONE', #5477, #2738 ) ;
#5411 = CARTESIAN_POINT ( 'NONE',  ( -12.24718835365690417, -4.666802875123986283, 33.22501703466257794 ) ) ;
#5412 = ORIENTED_EDGE ( 'NONE', *, *, #2518, .F. ) ;
#5413 = FACE_BOUND ( 'NONE', #5081, .T. ) ;
#5414 = ADVANCED_FACE ( 'NONE', ( #3622 ), #1267, .F. ) ;
#5415 = CARTESIAN_POINT ( 'NONE',  ( 9.833810162157899271, 3.423816715609354855, 25.60794618818621160 ) ) ;
#5416 = DIRECTION ( 'NONE',  ( -0.6273063437270228748, -0.7787725926866162496, 0.000000000000000000 ) ) ;
#5417 = EDGE_LOOP ( 'NONE', ( #2180, #5155, #5601, #4870 ) ) ;
#5418 = LINE ( 'NONE', #2102, #4123 ) ;
#5419 = EDGE_CURVE ( 'NONE', #6071, #6127, #4622, .T. ) ;
#5420 = CARTESIAN_POINT ( 'NONE',  ( 1.968147360634805443, -13.68731696136523546, 35.80501325620552677 ) ) ;
#5421 = ORIENTED_EDGE ( 'NONE', *, *, #1322, .F. ) ;
#5422 = CARTESIAN_POINT ( 'NONE',  ( 0.000000000000000000, 0.000000000000000000, 38.99999999999995737 ) ) ;
#5423 = VECTOR ( 'NONE', #1922, 1000.000000000000000 ) ;
#5424 = VERTEX_POINT ( 'NONE', #5571 ) ;
#5425 = LINE ( 'NONE', #264, #5159 ) ;
#5426 = CIRCLE ( 'NONE', #4936, 12.49999999999999822 ) ;
#5427 = LINE ( 'NONE', #2532, #100 ) ;
#5428 = CONTEXT_DEPENDENT_SHAPE_REPRESENTATION ( #4813, #4828 ) ;
#5429 = DIRECTION ( 'NONE',  ( 0.000000000000000000, 0.000000000000000000, 1.000000000000000000 ) ) ;
#5430 = CARTESIAN_POINT ( 'NONE',  ( 0.000000000000000000, 0.000000000000000000, 205.0000000000000568 ) ) ;
#5431 = AXIS2_PLACEMENT_3D ( 'NONE', #2817, #2354, #4245 ) ;
#5432 = VECTOR ( 'NONE', #2514, 1000.000000000000000 ) ;
#5433 = ORIENTED_EDGE ( 'NONE', *, *, #2781, .T. ) ;
#5434 = DIRECTION ( 'NONE',  ( -0.000000000000000000, -0.000000000000000000, -1.000000000000000000 ) ) ;
#5435 = CARTESIAN_POINT ( 'NONE',  ( 9.902916272933978803, 1.657983872361815658, 22.73823205004162418 ) ) ;
#5437 = CIRCLE ( 'NONE', #4120, 15.67638808697555142 ) ;
#5436 = DIRECTION ( 'NONE',  ( 0.000000000000000000, 0.000000000000000000, 1.000000000000000000 ) ) ;
#5438 = AXIS2_PLACEMENT_3D ( 'NONE', #4402, #507, #1877 ) ;
#5439 = VECTOR ( 'NONE', #5622, 1000.000000000000000 ) ;
#5440 = ORIENTED_EDGE ( 'NONE', *, *, #5471, .F. ) ;
#5441 = ADVANCED_FACE ( 'NONE', ( #1296 ), #4982, .F. ) ;
#5442 = LINE ( 'NONE', #3005, #5918 ) ;
#5443 = CARTESIAN_POINT ( 'NONE',  ( -8.965668681055127820, 0.8304760625349917325, 23.09216300389307719 ) ) ;
#5444 = VERTEX_POINT ( 'NONE', #4279 ) ;
#5445 = AXIS2_PLACEMENT_3D ( 'NONE', #5509, #4116, #6091 ) ;
#5446 = CARTESIAN_POINT ( 'NONE',  ( -9.245260337044125976, 9.269614772507654976, 25.40693856330804223 ) ) ;
#5447 = DIRECTION ( 'NONE',  ( -1.000000000000000000, 0.000000000000000000, 0.000000000000000000 ) ) ;
#5448 = EDGE_CURVE ( 'NONE', #1345, #5582, #6092, .T. ) ;
#5449 = ADVANCED_FACE ( 'NONE', ( #4756 ), #510, .F. ) ;
#5450 = CARTESIAN_POINT ( 'NONE',  ( 9.638809746143360613, 5.954763795926134584, 25.54536317066255791 ) ) ;
#5451 = AXIS2_PLACEMENT_3D ( 'NONE', #2964, #2471, #4362 ) ;
#5452 = DIRECTION ( 'NONE',  ( 1.000000000000000000, 0.000000000000000000, 0.000000000000000000 ) ) ;
#5453 = ORIENTED_EDGE ( 'NONE', *, *, #1081, .F. ) ;
#5454 = CARTESIAN_POINT ( 'NONE',  ( -6.000509662810409317, 9.000000000000001776, 23.13502399099478524 ) ) ;
#5455 = EDGE_CURVE ( 'NONE', #506, #6119, #4526, .T. ) ;
#5456 = FACE_BOUND ( 'NONE', #4085, .T. ) ;
#5457 = CIRCLE ( 'NONE', #3352, 12.50000000000138556 ) ;
#5458 = EDGE_CURVE ( 'NONE', #2297, #4386, #2614, .T. ) ;
#5459 = CARTESIAN_POINT ( 'NONE',  ( -2.654236408786764034, -10.78034266696900367, 28.16346921039841789 ) ) ;
#5460 = VERTEX_POINT ( 'NONE', #4714 ) ;
#5461 = CARTESIAN_POINT ( 'NONE',  ( 5.141101056459331353, 67.50000000000000000, 19.00000000000000000 ) ) ;
#5462 = AXIS2_PLACEMENT_3D ( 'NONE', #4164, #3694, #3207 ) ;
#5463 = EDGE_LOOP ( 'NONE', ( #520, #3168, #5058, #5304 ) ) ;
#5464 = DIRECTION ( 'NONE',  ( -1.000000000000000000, 0.000000000000000000, 0.000000000000000000 ) ) ;
#5465 = DIRECTION ( 'NONE',  ( -0.000000000000000000, -0.000000000000000000, -1.000000000000000000 ) ) ;
#5466 = APPLICATION_PROTOCOL_DEFINITION ( 'draft international standard', 'automotive_design', 1998, #40 ) ;
#5467 = VECTOR ( 'NONE', #5108, 1000.000000000000227 ) ;
#5468 = CARTESIAN_POINT ( 'NONE',  ( 58.45671475544921947, 33.75000000000068212, -35.00000000000000000 ) ) ;
#5469 = DIRECTION ( 'NONE',  ( 0.000000000000000000, 0.000000000000000000, -1.000000000000000000 ) ) ;
#5470 = CIRCLE ( 'NONE', #5367, 5.000000000000003553 ) ;
#5471 = EDGE_CURVE ( 'NONE', #4471, #3966, #1341, .T. ) ;
#5472 = ORIENTED_EDGE ( 'NONE', *, *, #208, .F. ) ;
#5473 = CARTESIAN_POINT ( 'NONE',  ( 7.077172123266715964, 10.77715421822219355, 30.61076540981938976 ) ) ;
#5474 = CARTESIAN_POINT ( 'NONE',  ( 15.67638808697554431, 1.082228759108213367, 38.00000000000000000 ) ) ;
#5475 = DIRECTION ( 'NONE',  ( 1.000000000000000000, 0.000000000000000000, 0.000000000000000000 ) ) ;
#5476 = ORIENTED_EDGE ( 'NONE', *, *, #5486, .T. ) ;
#5477 = CARTESIAN_POINT ( 'NONE',  ( 50.91502622129181788, 12.00000000000000355, 35.00000000000000000 ) ) ;
#5478 = CARTESIAN_POINT ( 'NONE',  ( -9.462636878983097688, 7.610208295502505216, 25.48187184588751464 ) ) ;
#5479 = ORIENTED_EDGE ( 'NONE', *, *, #4495, .T. ) ;
#5480 = CARTESIAN_POINT ( 'NONE',  ( -10.38144361273100458, 10.38144361273100635, 38.10175261887127363 ) ) ;
#5481 = LINE ( 'NONE', #5976, #573 ) ;
#5482 = CARTESIAN_POINT ( 'NONE',  ( 12.64046943599297101, 7.570233152424905576, 38.23931941266579315 ) ) ;
#5483 = FACE_OUTER_BOUND ( 'NONE', #2624, .T. ) ;
#5484 = ORIENTED_EDGE ( 'NONE', *, *, #3500, .T. ) ;
#5485 = CARTESIAN_POINT ( 'NONE',  ( -8.309552794738946702, 9.958856949317492990, 22.73823205004162418 ) ) ;
#5486 = EDGE_CURVE ( 'NONE', #3675, #1974, #3317, .T. ) ;
#5487 = CARTESIAN_POINT ( 'NONE',  ( -9.999999999999998224, 9.999999999999998224, 23.00000000000000000 ) ) ;
#5488 = CARTESIAN_POINT ( 'NONE',  ( -0.8880320553140829132, -10.89081796499577237, 28.17941898721253935 ) ) ;
#5489 = ORIENTED_EDGE ( 'NONE', *, *, #5841, .F. ) ;
#5490 = CARTESIAN_POINT ( 'NONE',  ( -12.49999999999999822, 67.50000000000000000, 19.00000000000001066 ) ) ;
#5491 = VERTEX_POINT ( 'NONE', #5623 ) ;
#5492 = CARTESIAN_POINT ( 'NONE',  ( 0.000000000000000000, 67.50000000000000000, 20.00000000000000000 ) ) ;
#5493 = CARTESIAN_POINT ( 'NONE',  ( 55.71784976887403928, 21.55374571496248137, -35.00000000000000000 ) ) ;
#5494 = APPLICATION_PROTOCOL_DEFINITION ( 'draft international standard', 'automotive_design', 1998, #161 ) ;
#5495 = ADVANCED_FACE ( 'NONE', ( #6123 ), #4687, .F. ) ;
#5496 = CARTESIAN_POINT ( 'NONE',  ( -1.301042606982566193E-13, 14.99999999999956124, 35.00000000000000000 ) ) ;
#5497 = FACE_OUTER_BOUND ( 'NONE', #2599, .T. ) ;
#5498 = VERTEX_POINT ( 'NONE', #5661 ) ;
#5499 = CARTESIAN_POINT ( 'NONE',  ( 10.27356722921338772, 10.12138240269938905, 35.55812462721154787 ) ) ;
#5500 = DIRECTION ( 'NONE',  ( 1.000000000000000000, 0.000000000000000000, 0.000000000000000000 ) ) ;
#5501 = DIRECTION ( 'NONE',  ( -0.6273063437270329779, 0.7787725926866080339, 0.000000000000000000 ) ) ;
#5502 = EDGE_CURVE ( 'NONE', #2370, #3250, #5332, .T. ) ;
#5503 = VERTEX_POINT ( 'NONE', #470 ) ;
#5504 = LINE ( 'NONE', #697, #258 ) ;
#5505 = CARTESIAN_POINT ( 'NONE',  ( -11.12726264164139600, 8.926511697459378780, 35.63515070857870626 ) ) ;
#5506 = ORIENTED_EDGE ( 'NONE', *, *, #5377, .F. ) ;
#5507 = FACE_BOUND ( 'NONE', #2498, .T. ) ;
#5508 = PRESENTATION_STYLE_ASSIGNMENT (( #3590 ) ) ;
#5509 = CARTESIAN_POINT ( 'NONE',  ( 52.58482424179591419, -72.37680137756305498, -40.00000000000000000 ) ) ;
#5510 = CARTESIAN_POINT ( 'NONE',  ( -9.074396217167167933, -58.26942451214404173, 35.00000000000000000 ) ) ;
#5511 = CARTESIAN_POINT ( 'NONE',  ( -8.333333333333316162, 9.999999999999998224, 23.00000000000000000 ) ) ;
#5512 = CARTESIAN_POINT ( 'NONE',  ( -5.113933401365549081, -9.708537589994012507, 25.56820946177495912 ) ) ;
#5513 = ORIENTED_EDGE ( 'NONE', *, *, #48, .T. ) ;
#5514 = CARTESIAN_POINT ( 'NONE',  ( -8.999999999999992895, -6.000509662810403100, 23.13502399099456142 ) ) ;
#5515 = ORIENTED_EDGE ( 'NONE', *, *, #3039, .T. ) ;
#5516 = FACE_OUTER_BOUND ( 'NONE', #3735, .T. ) ;
#5517 = FACE_OUTER_BOUND ( 'NONE', #4767, .T. ) ;
#5518 = CARTESIAN_POINT ( 'NONE',  ( -8.056095891487838412E-14, 1.254589464284425060E-14, 35.00000000000000000 ) ) ;
#5519 = CARTESIAN_POINT ( 'NONE',  ( -9.930636381741159369, -5.809855716632609024, 22.73823205004162418 ) ) ;
#5520 = VECTOR ( 'NONE', #1758, 1000.000000000000000 ) ;
#5521 = EDGE_CURVE ( 'NONE', #3966, #4001, #3221, .T. ) ;
#5522 = EDGE_CURVE ( 'NONE', #1135, #3734, #3929, .T. ) ;
#5523 = ORIENTED_EDGE ( 'NONE', *, *, #6011, .F. ) ;
#5524 = DIRECTION ( 'NONE',  ( 1.000000000000000000, 0.000000000000000000, 0.000000000000000000 ) ) ;
#5525 = CARTESIAN_POINT ( 'NONE',  ( -52.58482424179536707, 72.37680137756343868, -40.00000000000000000 ) ) ;
#5526 = CARTESIAN_POINT ( 'NONE',  ( -7.333173243373228622, 12.74975250248360936, 38.12600698484704509 ) ) ;
#5527 = DIRECTION ( 'NONE',  ( -0.4999999999999919509, -0.8660254037844432595, 0.000000000000000000 ) ) ;
#5528 = CIRCLE ( 'NONE', #1436, 10.00000000000000711 ) ;
#5529 = AXIS2_PLACEMENT_3D ( 'NONE', #979, #3358, #5669 ) ;
#5530 = ORIENTED_EDGE ( 'NONE', *, *, #2250, .T. ) ;
#5531 = CARTESIAN_POINT ( 'NONE',  ( 13.11522978513662707, -6.737147714782516950, 38.26633100282688105 ) ) ;
#5532 = EDGE_CURVE ( 'NONE', #3836, #4001, #411, .T. ) ;
#5533 = EDGE_CURVE ( 'NONE', #1649, #5376, #3817, .T. ) ;
#5534 = CARTESIAN_POINT ( 'NONE',  ( -9.933255351449997050, 9.419333092093008730, 30.50691708577705796 ) ) ;
#5535 = ORIENTED_EDGE ( 'NONE', *, *, #41, .T. ) ;
#5536 = CARTESIAN_POINT ( 'NONE',  ( -9.322893336083152960, 9.590870124851306855, 27.95908392747358917 ) ) ;
#5537 = CARTESIAN_POINT ( 'NONE',  ( 0.000000000000000000, 0.000000000000000000, 35.00000000000000000 ) ) ;
#5538 = B_SPLINE_SURFACE_WITH_KNOTS ( 'NONE', 3, 3, ( 
 ( #4310, #613, #1388, #2492, #3381, #6126, #1848 ),
 ( #514, #2391, #3745, #2820, #1419, #4281, #4720 ),
 ( #5692, #3318, #1154, #754, #1212, #3075, #3102 ),
 ( #5821, #3972, #5914, #4950, #2040, #3999, #2009 ),
 ( #5482, #1628, #1545, #3477, #3534, #3564, #4981 ),
 ( #2072, #3010, #1604, #5009, #4409, #5450, #1182 ),
 ( #728, #2610, #4500, #2129, #254, #702, #4027 ),
 ( #1130, #4473, #5947, #4894, #3940, #5858, #3501 ),
 ( #4379, #3904, #642, #3447, #2582, #5415, #5357 ),
 ( #1105, #196, #3041, #2984, #226, #2521, #156 ),
 ( #1578, #4919, #669, #2552, #4441, #6082, #2779 ),
 ( #5153, #5562, #2716, #427, #4676, #3644, #4646 ),
 ( #3185, #2306, #5183, #2749, #1286, #1312, #4614 ),
 ( #1746, #814, #369, #4143, #2277, #4170, #3157 ),
 ( #399, #5997, #1711, #5094, #840, #5650, #341 ),
 ( #3612, #4195, #5611, #6112, #1342, #2247, #6057 ),
 ( #3213, #1375, #1778, #2216, #3673, #1803, #314 ),
 ( #3279, #865, #3699, #4107, #3248, #900, #5587 ),
 ( #5119, #1831, #3732, #925, #4557, #2192, #4083 ),
 ( #5531, #1259, #5065, #2689, #4588, #6026, #2475 ),
 ( #2839, #3793, #1502, #1407, #3306, #3827, #3398 ),
 ( #4330, #1964, #3864, #595, #1053, #3370, #2436 ),
 ( #3892, #2379, #2931, #4779, #4744, #1870, #5808 ),
 ( #5343, #5746, #4842, #532, #497, #2410, #4366 ),
 ( #116, #4298, #47, #5240, #1926, #5781, #5310 ) ),
 .UNSPECIFIED., .F., .F., .F.,
 ( 4, 3, 3, 3, 3, 3, 3, 3, 4 ),
 ( 4, 3, 4 ),
 ( 0.000000000000000000, 0.1250000000000000000, 0.2500000000000000000, 0.3750000000000000000, 0.5000000000000000000, 0.6250000000000000000, 0.7500000000000000000, 0.8750000000000000000, 1.000000000000000000 ),
 ( 0.000000000000000000, 0.5087255983319458608, 1.017451196663891722 ),
 .UNSPECIFIED. ) ;
#5539 = CARTESIAN_POINT ( 'NONE',  ( 27.60043906316099083, 27.60043906316109386, 35.00000000000000000 ) ) ;
#5540 = CIRCLE ( 'NONE', #4328, 12.50000000000138911 ) ;
#5541 = CARTESIAN_POINT ( 'NONE',  ( -55.00000000000000711, -2.463307335887066074E-13, 35.00000000000000000 ) ) ;
#5542 = DIRECTION ( 'NONE',  ( 0.3607836771741465554, 0.9326495259660518844, -0.000000000000000000 ) ) ;
#5543 = ORIENTED_EDGE ( 'NONE', *, *, #3591, .T. ) ;
#5544 = VECTOR ( 'NONE', #1237, 1000.000000000000000 ) ;
#5545 = CARTESIAN_POINT ( 'NONE',  ( -5.390571672161876826, -11.22195964661421819, 30.65936073406735218 ) ) ;
#5546 = ORIENTED_EDGE ( 'NONE', *, *, #2743, .T. ) ;
#5547 = CARTESIAN_POINT ( 'NONE',  ( -11.99999999999999645, 12.00000000000000355, 20.00000000000000000 ) ) ;
#5548 = EDGE_LOOP ( 'NONE', ( #1503, #631 ) ) ;
#5549 = CARTESIAN_POINT ( 'NONE',  ( 58.45671475544921947, 33.75000000000068212, 35.00000000000000000 ) ) ;
#5550 = PLANE ( 'NONE',  #4647 ) ;
#5551 = AXIS2_PLACEMENT_3D ( 'NONE', #1223, #4393, #5399 ) ;
#5552 = DIRECTION ( 'NONE',  ( -0.000000000000000000, -0.000000000000000000, 1.000000000000000000 ) ) ;
#5553 = CARTESIAN_POINT ( 'NONE',  ( -9.902916272933978803, -1.657983872361813660, 22.73823205004162418 ) ) ;
#5554 = LINE ( 'NONE', #3180, #2865 ) ;
#5555 = AXIS2_PLACEMENT_3D ( 'NONE', #1765, #1220, #4160 ) ;
#5556 = ORIENTED_EDGE ( 'NONE', *, *, #1788, .T. ) ;
#5557 = CARTESIAN_POINT ( 'NONE',  ( -52.58482424179695158, -72.37680137756228760, -79.99999999999998579 ) ) ;
#5558 = CARTESIAN_POINT ( 'NONE',  ( -57.58482424179695869, -72.37680137756228760, -40.00000000000000000 ) ) ;
#5559 = CARTESIAN_POINT ( 'NONE',  ( 3.819063922342337047, 14.20304409106728727, 38.16887386538297733 ) ) ;
#5560 = EDGE_CURVE ( 'NONE', #5943, #2132, #5931, .T. ) ;
#5561 = ADVANCED_FACE ( 'NONE', ( #1 ), #4586, .T. ) ;
#5562 = CARTESIAN_POINT ( 'NONE',  ( 13.77854189090673387, 0.9833031778629049979, 35.81030296219172726 ) ) ;
#5563 = CARTESIAN_POINT ( 'NONE',  ( -9.269614772507654976, 9.245260337044141963, 25.40693856330804223 ) ) ;
#5564 = ORIENTED_EDGE ( 'NONE', *, *, #2629, .T. ) ;
#5565 = CARTESIAN_POINT ( 'NONE',  ( -3.322926169935024987, 8.964120776013636771, 23.06129021161080317 ) ) ;
#5566 = CARTESIAN_POINT ( 'NONE',  ( 80.08403291566592941, 27.64547812922851833, 40.00000000000000000 ) ) ;
#5567 = ADVANCED_FACE ( 'NONE', ( #2884 ), #4787, .T. ) ;
#5568 = CARTESIAN_POINT ( 'NONE',  ( 5.114554293134526134E-14, 6.349488965209711204E-14, -35.00000000000000000 ) ) ;
#5569 = CIRCLE ( 'NONE', #1871, 55.00000000000002132 ) ;
#5570 = LINE ( 'NONE', #5541, #5439 ) ;
#5571 = CARTESIAN_POINT ( 'NONE',  ( 9.074396217167732814, -58.26942451214393515, 35.00000000000000000 ) ) ;
#5572 = EDGE_CURVE ( 'NONE', #5747, #2322, #4213, .T. ) ;
#5573 = CARTESIAN_POINT ( 'NONE',  ( -8.662453428863081228, -10.23348454756166070, 30.54531259719474079 ) ) ;
#5574 = VERTEX_POINT ( 'NONE', #3875 ) ;
#5575 = DIRECTION ( 'NONE',  ( 0.3607836771741465554, 0.9326495259660518844, -0.000000000000000000 ) ) ;
#5576 = ORIENTED_EDGE ( 'NONE', *, *, #1129, .T. ) ;
#5577 = DIRECTION ( 'NONE',  ( -0.000000000000000000, -0.000000000000000000, -1.000000000000000000 ) ) ;
#5578 = CARTESIAN_POINT ( 'NONE',  ( 100.0000000000000000, 0.000000000000000000, -39.00000000000002842 ) ) ;
#5579 = CARTESIAN_POINT ( 'NONE',  ( -62.30180741492871022, -50.18450749816254586, 38.99999999999995737 ) ) ;
#5580 = CARTESIAN_POINT ( 'NONE',  ( -15.12434353048566571, 4.260267006495016773, 38.00000000000000711 ) ) ;
#5581 = DIRECTION ( 'NONE',  ( -0.7787725926866115866, 0.6273063437270286480, 0.000000000000000000 ) ) ;
#5582 = VERTEX_POINT ( 'NONE', #1944 ) ;
#5583 = CARTESIAN_POINT ( 'NONE',  ( -58.45671475544968843, 33.74999999999987210, 35.00000000000000000 ) ) ;
#5584 = DIRECTION ( 'NONE',  ( -0.000000000000000000, -0.000000000000000000, 1.000000000000000000 ) ) ;
#5585 = CARTESIAN_POINT ( 'NONE',  ( 6.075059976386698146, 13.36876581604897574, 38.14410695834214948 ) ) ;
#5586 =( NAMED_UNIT ( * ) SI_UNIT ( $, .STERADIAN. ) SOLID_ANGLE_UNIT ( ) );
#5587 = CARTESIAN_POINT ( 'NONE',  ( 8.963431154120575783, -4.154433491267528034, 23.04275521548131067 ) ) ;
#5588 = CARTESIAN_POINT ( 'NONE',  ( -12.64059746256322647, 7.570044180282075708, 38.23931193745812607 ) ) ;
#5589 = ORIENTED_EDGE ( 'NONE', *, *, #5347, .T. ) ;
#5590 = CARTESIAN_POINT ( 'NONE',  ( -8.785602912694963962, 10.67327843797381171, 33.09221060678261495 ) ) ;
#5591 = CARTESIAN_POINT ( 'NONE',  ( -1.131281550719566266E-13, -1.761763928569765259E-14, -35.00000000000000000 ) ) ;
#5592 = DIRECTION ( 'NONE',  ( 1.000000000000000000, 0.000000000000000000, 0.000000000000000000 ) ) ;
#5593 = CARTESIAN_POINT ( 'NONE',  ( 45.92560378283317135, -36.99336990414376913, 35.00000000000000000 ) ) ;
#5594 = ADVANCED_FACE ( 'NONE', ( #5790 ), #1543, .F. ) ;
#5595 = CARTESIAN_POINT ( 'NONE',  ( -72.00000000000004263, 0.000000000000000000, 45.00000000000000711 ) ) ;
#5596 = SHAPE_REPRESENTATION ( 'tube', ( #73 ), #684 ) ;
#5597 = CARTESIAN_POINT ( 'NONE',  ( -7.732441893382042686, -9.977717576970372093, 28.03187055541260264 ) ) ;
#5598 = ADVANCED_FACE ( 'NONE', ( #5355 ), #5620, .T. ) ;
#5599 = ORIENTED_EDGE ( 'NONE', *, *, #2324, .T. ) ;
#5600 = FACE_OUTER_BOUND ( 'NONE', #3845, .T. ) ;
#5601 = ORIENTED_EDGE ( 'NONE', *, *, #138, .F. ) ;
#5602 = DIRECTION ( 'NONE',  ( 0.7071067811865469066, 0.7071067811865482389, 0.000000000000000000 ) ) ;
#5603 = DIRECTION ( 'NONE',  ( -0.000000000000000000, 0.000000000000000000, 1.000000000000000000 ) ) ;
#5604 = CARTESIAN_POINT ( 'NONE',  ( 11.33314185116896589, 72.77350886803867525, -35.00000000000000000 ) ) ;
#5605 = CARTESIAN_POINT ( 'NONE',  ( -9.958856949317492990, 8.309552794738976900, 22.73823205004162418 ) ) ;
#5606 = CARTESIAN_POINT ( 'NONE',  ( 85.08403291566592941, 27.64547812922851833, -40.00000000000000000 ) ) ;
#5607 = ORIENTED_EDGE ( 'NONE', *, *, #3500, .F. ) ;
#5608 = CARTESIAN_POINT ( 'NONE',  ( -12.00000000000000000, 0.000000000000000000, 20.00000000000000000 ) ) ;
#5609 = CARTESIAN_POINT ( 'NONE',  ( 50.91502622129181788, 0.000000000000000000, 35.00000000000000000 ) ) ;
#5610 = CARTESIAN_POINT ( 'NONE',  ( 7.182140071210238271E-14, -8.916303653273167033E-14, 35.00000000000000000 ) ) ;
#5611 = CARTESIAN_POINT ( 'NONE',  ( 12.60026679007841643, -2.830884587392778595, 33.25110354061416729 ) ) ;
#5612 = VECTOR ( 'NONE', #308, 1000.000000000000000 ) ;
#5613 = CARTESIAN_POINT ( 'NONE',  ( -10.12138240269938727, 10.27356722921339127, 35.55812462721154787 ) ) ;
#5614 = ORIENTED_EDGE ( 'NONE', *, *, #3645, .T. ) ;
#5615 = DIRECTION ( 'NONE',  ( -1.000000000000000000, 0.000000000000000000, 0.000000000000000000 ) ) ;
#5616 = AXIS2_PLACEMENT_3D ( 'NONE', #5989, #3603, #804 ) ;
#5617 = EDGE_CURVE ( 'NONE', #1135, #5804, #3161, .T. ) ;
#5618 = ORIENTED_EDGE ( 'NONE', *, *, #2208, .T. ) ;
#5619 = FACE_OUTER_BOUND ( 'NONE', #1623, .T. ) ;
#5620 = CONICAL_SURFACE ( 'NONE', #2939, 100.0000000000000000, 0.7853981633974621568 ) ;
#5621 = TOROIDAL_SURFACE ( 'NONE', #2940, 5.141101056459331353, 10.00000000000000000 ) ;
#5622 = DIRECTION ( 'NONE',  ( -4.496403249731883200E-15, 1.000000000000000000, 0.000000000000000000 ) ) ;
#5623 = CARTESIAN_POINT ( 'NONE',  ( -45.92560378283290845, 36.99336990414408888, -35.00000000000000000 ) ) ;
#5624 = AXIS2_PLACEMENT_3D ( 'NONE', #4941, #5002, #3121 ) ;
#5625 = ADVANCED_FACE ( 'NONE', ( #2694 ), #1602, .T. ) ;
#5626 = EDGE_CURVE ( 'NONE', #5444, #1185, #1250, .T. ) ;
#5627 = CARTESIAN_POINT ( 'NONE',  ( -9.994658916190592990, -8.983694681928700021, 22.80938439471026058 ) ) ;
#5628 =( NAMED_UNIT ( * ) PLANE_ANGLE_UNIT ( ) SI_UNIT ( $, .RADIAN. ) );
#5629 = ORIENTED_EDGE ( 'NONE', *, *, #1972, .F. ) ;
#5630 = PLANE ( 'NONE',  #377 ) ;
#5631 = ORIENTED_EDGE ( 'NONE', *, *, #1398, .F. ) ;
#5632 = CYLINDRICAL_SURFACE ( 'NONE', #1730, 5.000000000000004441 ) ;
#5633 = AXIS2_PLACEMENT_3D ( 'NONE', #4664, #4094, #1762 ) ;
#5634 = CARTESIAN_POINT ( 'NONE',  ( 45.92560378283317135, -36.99336990414376913, 35.00000000000000000 ) ) ;
#5635 = CYLINDRICAL_SURFACE ( 'NONE', #5529, 12.50000000000139266 ) ;
#5636 = ORIENTED_EDGE ( 'NONE', *, *, #3455, .T. ) ;
#5637 = EDGE_CURVE ( 'NONE', #5798, #1401, #5071, .T. ) ;
#5638 = CARTESIAN_POINT ( 'NONE',  ( 50.91502622129181788, 15.00000000000000355, -35.00000000000000000 ) ) ;
#5639 = VECTOR ( 'NONE', #2091, 999.9999999999998863 ) ;
#5640 = CARTESIAN_POINT ( 'NONE',  ( 10.37777353962609972, -10.37777353962564852, 38.05103295300747845 ) ) ;
#5641 = ORIENTED_EDGE ( 'NONE', *, *, #4383, .F. ) ;
#5642 = CARTESIAN_POINT ( 'NONE',  ( 0.000000000000000000, 0.000000000000000000, 35.00000000000000000 ) ) ;
#5643 = DIRECTION ( 'NONE',  ( 1.000000000000000000, 0.000000000000000000, 0.000000000000000000 ) ) ;
#5644 = CARTESIAN_POINT ( 'NONE',  ( -8.540366387015959404, 11.94538915683136793, 38.10041598230911575 ) ) ;
#5645 = DIRECTION ( 'NONE',  ( 1.000000000000000000, 0.000000000000000000, 0.000000000000000000 ) ) ;
#5646 = AXIS2_PLACEMENT_3D ( 'NONE', #4994, #626, #142 ) ;
#5647 = TOROIDAL_SURFACE ( 'NONE', #3840, 5.141101056459331353, 10.00000000000000000 ) ;
#5648 = DIRECTION ( 'NONE',  ( -1.000000000000000000, -8.673617379884027583E-15, 0.000000000000000000 ) ) ;
#5649 = EDGE_CURVE ( 'NONE', #1046, #429, #5481, .T. ) ;
#5650 = CARTESIAN_POINT ( 'NONE',  ( 9.908812303639313868, -1.716658579843636678, 25.63028407385522911 ) ) ;
#5651 = AXIS2_PLACEMENT_3D ( 'NONE', #3908, #3242, #5090 ) ;
#5652 =( LENGTH_UNIT ( ) NAMED_UNIT ( * ) SI_UNIT ( .MILLI., .METRE. ) );
#5653 = ORIENTED_EDGE ( 'NONE', *, *, #5637, .T. ) ;
#5654 = AXIS2_PLACEMENT_3D ( 'NONE', #4609, #421, #4582 ) ;
#5655 = ORIENTED_EDGE ( 'NONE', *, *, #5112, .F. ) ;
#5656 = CARTESIAN_POINT ( 'NONE',  ( -5.114554293134481958E-14, -6.349488965209747807E-14, 35.00000000000000000 ) ) ;
#5657 = VECTOR ( 'NONE', #986, 1000.000000000000000 ) ;
#5658 = ORIENTED_EDGE ( 'NONE', *, *, #4805, .T. ) ;
#5659 = CARTESIAN_POINT ( 'NONE',  ( -47.58482424179695158, -72.37680137756228760, -40.00000000000000000 ) ) ;
#5660 = CARTESIAN_POINT ( 'NONE',  ( -9.269614772507654976, -9.245260337044127752, 25.40693856330804223 ) ) ;
#5661 = CARTESIAN_POINT ( 'NONE',  ( -90.08403291566611415, -27.64547812922793923, -40.00000000000000000 ) ) ;
#5662 = VECTOR ( 'NONE', #2559, 1000.000000000000000 ) ;
#5663 = LINE ( 'NONE', #5762, #3852 ) ;
#5664 = ORIENTED_EDGE ( 'NONE', *, *, #1155, .F. ) ;
#5665 = DIRECTION ( 'NONE',  ( 0.000000000000000000, 0.000000000000000000, 1.000000000000000000 ) ) ;
#5666 = ORIENTED_EDGE ( 'NONE', *, *, #215, .T. ) ;
#5667 = ADVANCED_FACE ( 'NONE', ( #2195 ), #3072, .F. ) ;
#5668 = LINE ( 'NONE', #580, #989 ) ;
#5669 = DIRECTION ( 'NONE',  ( -1.000000000000000000, 0.000000000000000000, 0.000000000000000000 ) ) ;
#5670 = ORIENTED_EDGE ( 'NONE', *, *, #5682, .F. ) ;
#5671 = DIRECTION ( 'NONE',  ( -0.000000000000000000, -0.000000000000000000, -1.000000000000000000 ) ) ;
#5672 = CARTESIAN_POINT ( 'NONE',  ( -74.61196207728390561, 28.86269417393235059, 38.99999999999995737 ) ) ;
#5673 = EDGE_LOOP ( 'NONE', ( #4692, #4226 ) ) ;
#5674 = ORIENTED_EDGE ( 'NONE', *, *, #334, .F. ) ;
#5675 = DIRECTION ( 'NONE',  ( -0.000000000000000000, 0.000000000000000000, 1.000000000000000000 ) ) ;
#5676 = EDGE_CURVE ( 'NONE', #915, #1920, #169, .T. ) ;
#5677 = FACE_OUTER_BOUND ( 'NONE', #323, .T. ) ;
#5678 =( NAMED_UNIT ( * ) PLANE_ANGLE_UNIT ( ) SI_UNIT ( $, .RADIAN. ) );
#5679 = CARTESIAN_POINT ( 'NONE',  ( 10.00265588554886165, 10.00265588554885632, 33.03935750738954624 ) ) ;
#5680 = FACE_OUTER_BOUND ( 'NONE', #1118, .T. ) ;
#5681 = ORIENTED_EDGE ( 'NONE', *, *, #2978, .T. ) ;
#5682 = EDGE_CURVE ( 'NONE', #1918, #4312, #160, .T. ) ;
#5683 = CARTESIAN_POINT ( 'NONE',  ( -6.736970939972922956, 13.11530391916999960, 38.26632377370044935 ) ) ;
#5684 = ORIENTED_EDGE ( 'NONE', *, *, #6012, .T. ) ;
#5685 = CARTESIAN_POINT ( 'NONE',  ( -55.00000000000000711, -2.463307335887066074E-13, 35.00000000000000000 ) ) ;
#5686 = PRODUCT_DEFINITION_SHAPE ( 'NONE', 'NONE',  #2955 ) ;
#5687 = ORIENTED_EDGE ( 'NONE', *, *, #2045, .T. ) ;
#5688 = CARTESIAN_POINT ( 'NONE',  ( 12.00215801354989154, -70.99259259259225985, 35.00000000000000000 ) ) ;
#5689 = LINE ( 'NONE', #2816, #4231 ) ;
#5690 = CARTESIAN_POINT ( 'NONE',  ( -13.37091851167933854, 6.070355506014839975, 38.14417062278695170 ) ) ;
#5691 = PRODUCT_DEFINITION_CONTEXT ( 'detailed design', #5128, 'design' ) ;
#5692 = CARTESIAN_POINT ( 'NONE',  ( 11.58129469348872931, 9.086808451283779675, 38.17632780249462598 ) ) ;
#5693 = CARTESIAN_POINT ( 'NONE',  ( -0.9766276285323429729, -14.65181115585165372, 38.18271774125523876 ) ) ;
#5694 = ORIENTED_EDGE ( 'NONE', *, *, #3998, .T. ) ;
#5695 = DIRECTION ( 'NONE',  ( 0.000000000000000000, 0.000000000000000000, 1.000000000000000000 ) ) ;
#5696 = LINE ( 'NONE', #5235, #3552 ) ;
#5697 = DIRECTION ( 'NONE',  ( -0.000000000000000000, -0.000000000000000000, 1.000000000000000000 ) ) ;
#5698 = EDGE_LOOP ( 'NONE', ( #298, #2941, #3059, #2035 ) ) ;
#5699 = CARTESIAN_POINT ( 'NONE',  ( 13.92731518891505438, -4.729006349282931509, 38.16144984630090420 ) ) ;
#5700 = CARTESIAN_POINT ( 'NONE',  ( 6.095798759547082390, -10.32656711695237739, 28.09297316833069402 ) ) ;
#5701 = ORIENTED_EDGE ( 'NONE', *, *, #2491, .T. ) ;
#5702 = ORIENTED_EDGE ( 'NONE', *, *, #4138, .T. ) ;
#5703 = LINE ( 'NONE', #3302, #5657 ) ;
#5704 = LINE ( 'NONE', #3762, #5356 ) ;
#5705 = CARTESIAN_POINT ( 'NONE',  ( 88.92935091904816147, 26.48012904884922136, 0.000000000000000000 ) ) ;
#5706 = CARTESIAN_POINT ( 'NONE',  ( 8.999999999988068211, 9.000000000000005329, 23.06137295785747554 ) ) ;
#5707 = DIRECTION ( 'NONE',  ( -0.000000000000000000, -0.000000000000000000, 1.000000000000000000 ) ) ;
#5708 = EDGE_CURVE ( 'NONE', #6071, #5369, #5911, .T. ) ;
#5709 = ADVANCED_FACE ( 'NONE', ( #2124 ), #4530, .F. ) ;
#5710 = EDGE_LOOP ( 'NONE', ( #3901, #3156, #1959, #2156 ) ) ;
#5711 = CARTESIAN_POINT ( 'NONE',  ( 5.685785403169734131, 12.74411457810409409, 35.74643938915853880 ) ) ;
#5712 = CARTESIAN_POINT ( 'NONE',  ( 5.809855716632679190, 9.930636381741159369, 22.73823205004162418 ) ) ;
#5713 = CARTESIAN_POINT ( 'NONE',  ( -13.74495680931371666, -5.167291852658159712, 38.15579506865710613 ) ) ;
#5714 = ORIENTED_EDGE ( 'NONE', *, *, #3493, .F. ) ;
#5715 = EDGE_CURVE ( 'NONE', #4988, #906, #1624, .T. ) ;
#5716 = DIRECTION ( 'NONE',  ( 0.8660254037844385966, -0.5000000000000001110, 0.000000000000000000 ) ) ;
#5717 = ADVANCED_FACE ( 'NONE', ( #5507, #3616, #3561, #4472, #3499, #1264, #5008, #5413, #3127, #753, #2634, #1151 ), #284, .F. ) ;
#5718 = CARTESIAN_POINT ( 'NONE',  ( -9.977717576970366764, -7.732441893382013376, 28.03187055541259554 ) ) ;
#5719 = VECTOR ( 'NONE', #838, 1000.000000000000000 ) ;
#5720 = DIRECTION ( 'NONE',  ( -0.000000000000000000, 0.000000000000000000, 1.000000000000000000 ) ) ;
#5721 = PRODUCT_DEFINITION_SHAPE ( 'NONE', 'NONE',  #6154 ) ;
#5722 = AXIS2_PLACEMENT_3D ( 'NONE', #5595, #934, #1320 ) ;
#5723 = CIRCLE ( 'NONE', #1153, 12.49999999999999822 ) ;
#5724 = DIRECTION ( 'NONE',  ( 0.000000000000000000, -0.000000000000000000, -1.000000000000000000 ) ) ;
#5725 = CARTESIAN_POINT ( 'NONE',  ( -1.937269431830245248, -14.55597330376941123, 38.18000980160655899 ) ) ;
#5726 = CIRCLE ( 'NONE', #5341, 72.00000000000004263 ) ;
#5727 = VERTEX_POINT ( 'NONE', #4565 ) ;
#5728 = DIRECTION ( 'NONE',  ( -0.000000000000000000, -0.000000000000000000, 1.000000000000000000 ) ) ;
#5729 = CIRCLE ( 'NONE', #3038, 12.50000000000138556 ) ;
#5730 = DIRECTION ( 'NONE',  ( 1.000000000000000000, 0.000000000000000000, 0.000000000000000000 ) ) ;
#5731 = CARTESIAN_POINT ( 'NONE',  ( 4.999999999999380940, -89.46264649666795776, -79.99999999999998579 ) ) ;
#5732 = EDGE_LOOP ( 'NONE', ( #2308, #4780, #1327, #1721 ) ) ;
#5733 = DIRECTION ( 'NONE',  ( -0.000000000000000000, 0.000000000000000000, 1.000000000000000000 ) ) ;
#5734 =( GEOMETRIC_REPRESENTATION_CONTEXT ( 3 ) GLOBAL_UNCERTAINTY_ASSIGNED_CONTEXT ( ( #1385 ) ) GLOBAL_UNIT_ASSIGNED_CONTEXT ( ( #5406, #691, #3064 ) ) REPRESENTATION_CONTEXT ( 'NONE', 'WORKASPACE' ) );
#5735 = CARTESIAN_POINT ( 'NONE',  ( 9.632247231687289357, -10.63625351335941538, 35.59852902770369099 ) ) ;
#5736 = CIRCLE ( 'NONE', #1351, 10.00000000000000178 ) ;
#5737 = VERTEX_POINT ( 'NONE', #6001 ) ;
#5738 = ADVANCED_FACE ( 'NONE', ( #1714 ), #6086, .F. ) ;
#5739 = ORIENTED_EDGE ( 'NONE', *, *, #1694, .F. ) ;
#5740 = LINE ( 'NONE', #526, #3959 ) ;
#5741 = CARTESIAN_POINT ( 'NONE',  ( -9.999999999999998224, 9.999999999999998224, -167.0000000000000284 ) ) ;
#5742 = PLANE ( 'NONE',  #4559 ) ;
#5743 = CARTESIAN_POINT ( 'NONE',  ( 0.000000000000000000, 0.000000000000000000, 0.000000000000000000 ) ) ;
#5744 = ADVANCED_BREP_SHAPE_REPRESENTATION ( '', ( #249, #73 ), #875 ) ;
#5745 = DIRECTION ( 'NONE',  ( 0.9326495259660421144, 0.3607836771741718129, 0.000000000000000000 ) ) ;
#5746 = CARTESIAN_POINT ( 'NONE',  ( 10.63625351335941538, -9.632247231687294686, 35.59852902770369809 ) ) ;
#5747 = VERTEX_POINT ( 'NONE', #5189 ) ;
#5748 = CARTESIAN_POINT ( 'NONE',  ( 2.780685750889414288E-14, 9.928243323025453648, 25.63579099555277807 ) ) ;
#5749 = CARTESIAN_POINT ( 'NONE',  ( 9.144590365090033757, 9.969668718019493170, 22.73823205004162418 ) ) ;
#5750 = LINE ( 'NONE', #3402, #3532 ) ;
#5751 = ADVANCED_FACE ( 'NONE', ( #2785 ), #6063, .F. ) ;
#5752 = ORIENTED_EDGE ( 'NONE', *, *, #2593, .T. ) ;
#5753 = CARTESIAN_POINT ( 'NONE',  ( 8.056095891487838412E-14, -1.254589464284425060E-14, 35.00000000000000000 ) ) ;
#5754 = VECTOR ( 'NONE', #4217, 1000.000000000000000 ) ;
#5755 = CARTESIAN_POINT ( 'NONE',  ( -10.27564057804868725, -9.515772848102848513, 33.05475024408053031 ) ) ;
#5756 = AXIS2_PLACEMENT_3D ( 'NONE', #1366, #2299, #835 ) ;
#5757 = VECTOR ( 'NONE', #3176, 1000.000000000000000 ) ;
#5758 = CARTESIAN_POINT ( 'NONE',  ( 5.833333333333301063, -9.999999999999998224, 23.00000000000000000 ) ) ;
#5759 = EDGE_CURVE ( 'NONE', #5893, #4711, #1733, .T. ) ;
#5760 = CIRCLE ( 'NONE', #3070, 5.000000000000004441 ) ;
#5761 = VECTOR ( 'NONE', #1049, 999.9999999999998863 ) ;
#5762 = CARTESIAN_POINT ( 'NONE',  ( -2.941541598353333735E-14, 7.604078429494112756E-14, 35.00000000000000000 ) ) ;
#5763 = CARTESIAN_POINT ( 'NONE',  ( 8.540366387015776439, -11.94538915683149582, 38.10041598230914417 ) ) ;
#5764 = CIRCLE ( 'NONE', #1001, 15.67638808697555142 ) ;
#5765 = EDGE_LOOP ( 'NONE', ( #6078, #1900, #6114, #2228 ) ) ;
#5766 = EDGE_CURVE ( 'NONE', #2468, #5369, #6117, .T. ) ;
#5767 = FACE_OUTER_BOUND ( 'NONE', #1409, .T. ) ;
#5768 = DIRECTION ( 'NONE',  ( -0.000000000000000000, -0.000000000000000000, 1.000000000000000000 ) ) ;
#5769 = ORIENTED_EDGE ( 'NONE', *, *, #4573, .F. ) ;
#5770 = FACE_BOUND ( 'NONE', #2645, .T. ) ;
#5771 = CARTESIAN_POINT ( 'NONE',  ( 7.228764404800513965, -11.39256393965315795, 33.15620429642044797 ) ) ;
#5772 = APPLICATION_CONTEXT ( 'automotive_design' ) ;
#5773 = VERTEX_POINT ( 'NONE', #844 ) ;
#5774 = CARTESIAN_POINT ( 'NONE',  ( -9.166555234036119160, 10.04707028972858929, 25.36260747786040071 ) ) ;
#5775 = EDGE_LOOP ( 'NONE', ( #126, #5244, #4435, #3104, #4562, #4902, #16 ) ) ;
#5776 = CARTESIAN_POINT ( 'NONE',  ( 47.58482424179642578, 72.37680137756268550, 40.00000000000000000 ) ) ;
#5777 = CARTESIAN_POINT ( 'NONE',  ( 0.000000000000000000, 0.000000000000000000, -167.0000000000000284 ) ) ;
#5778 = CARTESIAN_POINT ( 'NONE',  ( 30.10043906316099083, 27.60043906316109386, 35.00000000000000000 ) ) ;
#5779 = CARTESIAN_POINT ( 'NONE',  ( 0.000000000000000000, 0.000000000000000000, 0.000000000000000000 ) ) ;
#5780 = DIRECTION ( 'NONE',  ( -0.000000000000000000, -0.000000000000000000, -1.000000000000000000 ) ) ;
#5781 = CARTESIAN_POINT ( 'NONE',  ( 9.166555234036119160, -10.04707028972858929, 25.36260747786040071 ) ) ;
#5782 = VERTEX_POINT ( 'NONE', #3677 ) ;
#5783 = CARTESIAN_POINT ( 'NONE',  ( 3.645573174172184849, 11.58281169573756131, 30.69674159737795449 ) ) ;
#5784 = CARTESIAN_POINT ( 'NONE',  ( 8.333333333333348136, 9.999999999999998224, 23.00000000000000000 ) ) ;
#5785 = CARTESIAN_POINT ( 'NONE',  ( 0.000000000000000000, 0.000000000000000000, 38.99999999999995737 ) ) ;
#5786 = VERTEX_POINT ( 'NONE', #1945 ) ;
#5787 = DIRECTION ( 'NONE',  ( -0.000000000000000000, 0.000000000000000000, 1.000000000000000000 ) ) ;
#5788 = CARTESIAN_POINT ( 'NONE',  ( -11.58129469348872398, -9.086808451283777899, 38.17632780249461888 ) ) ;
#5789 = ORIENTED_EDGE ( 'NONE', *, *, #4206, .F. ) ;
#5790 = FACE_OUTER_BOUND ( 'NONE', #2516, .T. ) ;
#5791 = EDGE_CURVE ( 'NONE', #1495, #4773, #2690, .T. ) ;
#5792 = CARTESIAN_POINT ( 'NONE',  ( -3.000437278975514044, -9.000000000000001776, 23.18288419282211876 ) ) ;
#5793 = DIRECTION ( 'NONE',  ( 1.000000000000000000, 0.000000000000000000, 0.000000000000000000 ) ) ;
#5794 = VERTEX_POINT ( 'NONE', #4618 ) ;
#5795 = CARTESIAN_POINT ( 'NONE',  ( -12.49999999999999822, 67.50000000000000000, -19.00000000000000711 ) ) ;
#5796 = CARTESIAN_POINT ( 'NONE',  ( 9.999999999999998224, -9.999999999999998224, 23.00000000000000000 ) ) ;
#5797 = CARTESIAN_POINT ( 'NONE',  ( 15.00000000000000178, 52.91502622129183209, -35.00000000000000000 ) ) ;
#5798 = VERTEX_POINT ( 'NONE', #3285 ) ;
#5799 = EDGE_CURVE ( 'NONE', #4734, #1178, #930, .T. ) ;
#5800 = DIRECTION ( 'NONE',  ( 0.000000000000000000, 0.000000000000000000, 1.000000000000000000 ) ) ;
#5801 = ADVANCED_FACE ( 'NONE', ( #3703 ), #5220, .F. ) ;
#5802 = CARTESIAN_POINT ( 'NONE',  ( 7.487361748921619764, -8.967351122863068014, 22.92808036848186859 ) ) ;
#5803 = ORIENTED_EDGE ( 'NONE', *, *, #2567, .F. ) ;
#5804 = VERTEX_POINT ( 'NONE', #872 ) ;
#5805 = CARTESIAN_POINT ( 'NONE',  ( 90.08403291566575888, -27.64547812922912939, -79.99999999999998579 ) ) ;
#5806 = DIRECTION ( 'NONE',  ( 2.220446049250313081E-16, -1.000000000000000222, 6.660920792866264645E-17 ) ) ;
#5807 = CARTESIAN_POINT ( 'NONE',  ( -9.999999999999996447, -9.999999999999996447, 22.99999999999995737 ) ) ;
#5808 = CARTESIAN_POINT ( 'NONE',  ( 8.970286671637149212, -8.321939193476740826, 22.89273732682886475 ) ) ;
#5809 = ORIENTED_EDGE ( 'NONE', *, *, #4597, .F. ) ;
#5810 = CARTESIAN_POINT ( 'NONE',  ( -0.8304760625348921455, 8.965668681055129596, 23.09216300389309140 ) ) ;
#5811 = DIRECTION ( 'NONE',  ( 0.4999999999999976685, 0.8660254037844400399, 0.000000000000000000 ) ) ;
#5812 = CARTESIAN_POINT ( 'NONE',  ( 9.999999999999998224, 9.999999999999998224, 23.00000000000000000 ) ) ;
#5813 = VERTEX_POINT ( 'NONE', #5158 ) ;
#5814 = DIRECTION ( 'NONE',  ( -0.9326495259660493309, 0.3607836771741531612, 0.000000000000000000 ) ) ;
#5815 = CARTESIAN_POINT ( 'NONE',  ( -9.928243323025453648, 0.8581648076837686823, 25.63579099555280294 ) ) ;
#5816 = ORIENTED_EDGE ( 'NONE', *, *, #742, .F. ) ;
#5817 = PRODUCT_RELATED_PRODUCT_CATEGORY ( 'part', '', ( #1404 ) ) ;
#5818 = CARTESIAN_POINT ( 'NONE',  ( 3.333333333333289961, -9.999999999999998224, 23.00000000000000000 ) ) ;
#5819 = ADVANCED_BREP_SHAPE_REPRESENTATION ( '', ( #4119, #73 ), #684 ) ;
#5820 = AXIS2_PLACEMENT_3D ( 'NONE', #4971, #1566, #5380 ) ;
#5821 = CARTESIAN_POINT ( 'NONE',  ( 12.11088206474084927, 8.328520801854342182, 38.20782360758020957 ) ) ;
#5822 = CARTESIAN_POINT ( 'NONE',  ( 3.785572473853858089, -14.18798205797851075, 38.16905032409691501 ) ) ;
#5823 = EDGE_LOOP ( 'NONE', ( #4921, #4542, #2106, #6089, #446 ) ) ;
#5824 = DIRECTION ( 'NONE',  ( 1.000000000000000000, 0.000000000000000000, 0.000000000000000000 ) ) ;
#5825 = VECTOR ( 'NONE', #949, 1000.000000000000000 ) ;
#5826 = EDGE_CURVE ( 'NONE', #1202, #1681, #431, .T. ) ;
#5827 = AXIS2_PLACEMENT_3D ( 'NONE', #387, #2234, #2681 ) ;
#5828 = EDGE_CURVE ( 'NONE', #1252, #3886, #563, .T. ) ;
#5829 = PLANE ( 'NONE',  #4726 ) ;
#5830 = DIRECTION ( 'NONE',  ( 1.000000000000000000, 0.000000000000000000, 0.000000000000000000 ) ) ;
#5831 = PRODUCT_DEFINITION_SHAPE ( 'NONE', 'NONE',  #6143 ) ;
#5832 = CARTESIAN_POINT ( 'NONE',  ( 10.19494410001831142, -9.858401829237472214, 33.01259202755186095 ) ) ;
#5833 = AXIS2_PLACEMENT_3D ( 'NONE', #5537, #4592, #345 ) ;
#5834 = ORIENTED_EDGE ( 'NONE', *, *, #215, .F. ) ;
#5835 =( NAMED_UNIT ( * ) SI_UNIT ( $, .STERADIAN. ) SOLID_ANGLE_UNIT ( ) );
#5836 = ORIENTED_EDGE ( 'NONE', *, *, #1629, .F. ) ;
#5837 = CARTESIAN_POINT ( 'NONE',  ( -4.130675435985315210E-14, -1.067806758184287486E-13, 35.00000000000000000 ) ) ;
#5838 = ADVANCED_FACE ( 'NONE', ( #4681 ), #3736, .F. ) ;
#5839 = DIRECTION ( 'NONE',  ( -0.000000000000000000, -0.000000000000000000, -1.000000000000000000 ) ) ;
#5840 = DIRECTION ( 'NONE',  ( -0.8663988788866361368, 0.4993525634899455001, 0.000000000000000000 ) ) ;
#5841 = EDGE_CURVE ( 'NONE', #4037, #3906, #5726, .T. ) ;
#5842 = VECTOR ( 'NONE', #375, 1000.000000000000227 ) ;
#5843 = CARTESIAN_POINT ( 'NONE',  ( 11.33314185117008677, -72.77350886804093477, 35.00000000000000000 ) ) ;
#5844 = CARTESIAN_POINT ( 'NONE',  ( -12.50000000000155254, 67.50000000000002842, 35.00000000000000000 ) ) ;
#5845 =( LENGTH_UNIT ( ) NAMED_UNIT ( * ) SI_UNIT ( .MILLI., .METRE. ) );
#5846 = ORIENTED_EDGE ( 'NONE', *, *, #5572, .T. ) ;
#5847 = CARTESIAN_POINT ( 'NONE',  ( 27.50000000000000355, 47.63139720814412215, -35.00000000000000000 ) ) ;
#5848 = CARTESIAN_POINT ( 'NONE',  ( 15.56315586465742840, -2.164213882025735280, 38.00000000000002132 ) ) ;
#5849 = CARTESIAN_POINT ( 'NONE',  ( 85.08403291566592941, 27.64547812922851833, -79.99999999999998579 ) ) ;
#5850 = EDGE_CURVE ( 'NONE', #2489, #5243, #5098, .T. ) ;
#5851 = VERTEX_POINT ( 'NONE', #5566 ) ;
#5852 = DIRECTION ( 'NONE',  ( -1.000000000000000000, 0.000000000000000000, 0.000000000000000000 ) ) ;
#5853 = CARTESIAN_POINT ( 'NONE',  ( -14.74111653287705792, -1.016991241531516765, 38.35393095385146012 ) ) ;
#5854 = VERTEX_POINT ( 'NONE', #4174 ) ;
#5855 = CARTESIAN_POINT ( 'NONE',  ( -4.166666666666706931, -9.999999999999998224, 23.00000000000000000 ) ) ;
#5856 = CIRCLE ( 'NONE', #1090, 12.50000000000000355 ) ;
#5857 = MECHANICAL_DESIGN_GEOMETRIC_PRESENTATION_REPRESENTATION (  '', ( #3158 ), #803 ) ;
#5858 = CARTESIAN_POINT ( 'NONE',  ( 9.778265433844637755, 4.273103006804793935, 25.59105575288735324 ) ) ;
#5859 = AXIS2_PLACEMENT_3D ( 'NONE', #801, #2294, #4071 ) ;
#5860 = CARTESIAN_POINT ( 'NONE',  ( -67.48246767247867695, 25.10212255632726297, 35.00000000000000000 ) ) ;
#5861 = ORIENTED_EDGE ( 'NONE', *, *, #5897, .F. ) ;
#5862 = CARTESIAN_POINT ( 'NONE',  ( -52.58482424179695158, -72.37680137756228760, 40.00000000000000000 ) ) ;
#5863 = VECTOR ( 'NONE', #807, 1000.000000000000000 ) ;
#5864 = AXIS2_PLACEMENT_3D ( 'NONE', #235, #737, #141 ) ;
#5865 = AXIS2_PLACEMENT_3D ( 'NONE', #2400, #3360, #1460 ) ;
#5866 = CARTESIAN_POINT ( 'NONE',  ( -4.666652649023723676, -12.24723121994938957, 33.22501677959694177 ) ) ;
#5867 = ADVANCED_FACE ( 'NONE', ( #1412 ), #3238, .F. ) ;
#5868 = ORIENTED_EDGE ( 'NONE', *, *, #401, .T. ) ;
#5869 = CARTESIAN_POINT ( 'NONE',  ( -9.999999999999998224, -9.999999999999998224, 23.00000000000000000 ) ) ;
#5870 = ORIENTED_EDGE ( 'NONE', *, *, #2631, .T. ) ;
#5871 = CARTESIAN_POINT ( 'NONE',  ( 14.67638808697651953, 0.9595328539160939973, 38.18288438803428875 ) ) ;
#5872 = FACE_OUTER_BOUND ( 'NONE', #551, .T. ) ;
#5873 = VECTOR ( 'NONE', #1898, 1000.000000000000000 ) ;
#5874 = CARTESIAN_POINT ( 'NONE',  ( -45.92560378283290845, 36.99336990414408888, 35.00000000000000000 ) ) ;
#5875 = FACE_OUTER_BOUND ( 'NONE', #4376, .T. ) ;
#5876 = EDGE_CURVE ( 'NONE', #1165, #5015, #3824, .T. ) ;
#5877 = EDGE_LOOP ( 'NONE', ( #291, #6041, #4730, #5546 ) ) ;
#5878 = CARTESIAN_POINT ( 'NONE',  ( 8.328520801854336852, 12.11088206474084927, 38.20782360758020246 ) ) ;
#5879 = CARTESIAN_POINT ( 'NONE',  ( -27.50000000000010303, 47.63139720814406530, 35.00000000000000000 ) ) ;
#5880 = CARTESIAN_POINT ( 'NONE',  ( -90.08403291566611415, -27.64547812922793923, 40.00000000000000000 ) ) ;
#5881 = VERTEX_POINT ( 'NONE', #4149 ) ;
#5882 = DIRECTION ( 'NONE',  ( 1.000000000000000000, 0.000000000000000000, 0.000000000000000000 ) ) ;
#5883 = EDGE_CURVE ( 'NONE', #2261, #1931, #3720, .T. ) ;
#5884 = CARTESIAN_POINT ( 'NONE',  ( -8.965240827029074211, -1.660911000355771883, 23.08598180255751942 ) ) ;
#5885 = ORIENTED_EDGE ( 'NONE', *, *, #324, .T. ) ;
#5886 = CARTESIAN_POINT ( 'NONE',  ( -8.069545871843436302, -13.47611570251764768, 37.99999999999999289 ) ) ;
#5887 = PRODUCT_DEFINITION_SHAPE ( 'NONE', 'NONE',  #6155 ) ;
#5888 = LINE ( 'NONE', #3760, #5520 ) ;
#5889 = ORIENTED_EDGE ( 'NONE', *, *, #1333, .F. ) ;
#5890 = CARTESIAN_POINT ( 'NONE',  ( -57.35713647666923976, 46.20154318182412112, 35.13717928826270054 ) ) ;
#5891 = APPLICATION_CONTEXT ( 'automotive_design' ) ;
#5892 = CARTESIAN_POINT ( 'NONE',  ( 0.8304760625348978076, -8.965668681055127820, 23.09216300389306653 ) ) ;
#5893 = VERTEX_POINT ( 'NONE', #148 ) ;
#5894 = CARTESIAN_POINT ( 'NONE',  ( 0.000000000000000000, 67.50000000000000000, -28.99999999999999645 ) ) ;
#5895 = EDGE_LOOP ( 'NONE', ( #3077, #3449, #2320, #3066 ) ) ;
#5896 = CARTESIAN_POINT ( 'NONE',  ( 11.65565333135118209, 8.931668428567823170, 38.09186409098168014 ) ) ;
#5897 = EDGE_CURVE ( 'NONE', #1998, #5370, #2644, .T. ) ;
#5898 = DIRECTION ( 'NONE',  ( 0.9326495259660420034, 0.3607836771741718129, 0.000000000000000000 ) ) ;
#5899 = ITEM_DEFINED_TRANSFORMATION ( 'NONE', 'NONE', #4229,  #73 ) ;
#5900 = LINE ( 'NONE', #5874, #5075 ) ;
#5901 = CARTESIAN_POINT ( 'NONE',  ( -85.08403291566554572, 27.64547812922971914, 40.00000000000000000 ) ) ;
#5902 = EDGE_LOOP ( 'NONE', ( #869, #3869, #2718, #2292 ) ) ;
#5903 = CARTESIAN_POINT ( 'NONE',  ( -9.999999999999998224, 9.999999999999998224, -167.0000000000000284 ) ) ;
#5904 = CARTESIAN_POINT ( 'NONE',  ( 9.999999999999998224, 3.333333333333289961, 23.00000000000000000 ) ) ;
#5905 = ADVANCED_FACE ( 'NONE', ( #27 ), #1058, .F. ) ;
#5906 = EDGE_CURVE ( 'NONE', #4527, #1495, #4222, .T. ) ;
#5907 = ORIENTED_EDGE ( 'NONE', *, *, #1442, .T. ) ;
#5908 = CARTESIAN_POINT ( 'NONE',  ( 15.00000000000000178, 52.91502622129182498, 20.00000000000000000 ) ) ;
#5909 = CARTESIAN_POINT ( 'NONE',  ( -8.965668681055127820, 4.802124745462707424E-14, 23.09216300389307719 ) ) ;
#5910 = VERTEX_POINT ( 'NONE', #4337 ) ;
#5911 = LINE ( 'NONE', #4057, #1723 ) ;
#5912 = ADVANCED_FACE ( 'NONE', ( #2029 ), #4912, .F. ) ;
#5913 = EDGE_CURVE ( 'NONE', #3470, #4790, #1547, .T. ) ;
#5914 = CARTESIAN_POINT ( 'NONE',  ( 11.03292118881348394, 8.007183658747743848, 33.12420745160152791 ) ) ;
#5915 = CARTESIAN_POINT ( 'NONE',  ( 0.000000000000000000, 0.000000000000000000, 45.00000000000000711 ) ) ;
#5916 = VERTEX_POINT ( 'NONE', #5382 ) ;
#5917 = CARTESIAN_POINT ( 'NONE',  ( 3.000437278975559785, 9.000000000000003553, 23.18288419282210810 ) ) ;
#5918 = VECTOR ( 'NONE', #1176, 1000.000000000000000 ) ;
#5919 = CARTESIAN_POINT ( 'NONE',  ( 27.50000000000043698, -47.63139720814386635, -35.00000000000000000 ) ) ;
#5920 = CARTESIAN_POINT ( 'NONE',  ( -3.423848683943053750, -9.833809958618578762, 25.60794474275443022 ) ) ;
#5921 = ORIENTED_EDGE ( 'NONE', *, *, #1736, .T. ) ;
#5922 = DIRECTION ( 'NONE',  ( 0.000000000000000000, 0.000000000000000000, -1.000000000000000000 ) ) ;
#5923 = AXIS2_PLACEMENT_3D ( 'NONE', #4951, #3366, #554 ) ;
#5924 = ORIENTED_EDGE ( 'NONE', *, *, #6088, .F. ) ;
#5925 = CARTESIAN_POINT ( 'NONE',  ( 12.00000000000000000, 12.00000000000000355, -35.00000000000000000 ) ) ;
#5926 = VECTOR ( 'NONE', #2557, 1000.000000000000000 ) ;
#5927 = DIRECTION ( 'NONE',  ( -0.5000000000000042188, 0.8660254037844362651, 0.000000000000000000 ) ) ;
#5928 = APPLICATION_PROTOCOL_DEFINITION ( 'draft international standard', 'automotive_design', 1998, #4404 ) ;
#5929 = CARTESIAN_POINT ( 'NONE',  ( 0.000000000000000000, 0.000000000000000000, 38.00000000000000000 ) ) ;
#5930 = DIRECTION ( 'NONE',  ( 1.000000000000000000, 0.000000000000000000, 0.000000000000000000 ) ) ;
#5931 = CIRCLE ( 'NONE', #5431, 80.00000000000002842 ) ;
#5932 = VERTEX_POINT ( 'NONE', #5812 ) ;
#5933 = VECTOR ( 'NONE', #2253, 1000.000000000000000 ) ;
#5934 = ORIENTED_EDGE ( 'NONE', *, *, #1318, .F. ) ;
#5935 = CYLINDRICAL_SURFACE ( 'NONE', #1535, 5.000000000000004441 ) ;
#5936 = CARTESIAN_POINT ( 'NONE',  ( 9.900940235153617763, 0.8289898103093435999, 22.73823205004162773 ) ) ;
#5937 = LINE ( 'NONE', #4974, #3137 ) ;
#5938 = AXIS2_PLACEMENT_3D ( 'NONE', #645, #4382, #2012 ) ;
#5939 = ORIENTED_EDGE ( 'NONE', *, *, #4249, .F. ) ;
#5940 = PLANE ( 'NONE',  #277 ) ;
#5941 = DIRECTION ( 'NONE',  ( 0.000000000000000000, 0.000000000000000000, -1.000000000000000000 ) ) ;
#5942 = CARTESIAN_POINT ( 'NONE',  ( -10.78034266696899657, -2.654236408786700085, 28.16346921039841078 ) ) ;
#5943 = VERTEX_POINT ( 'NONE', #4276 ) ;
#5944 = EDGE_CURVE ( 'NONE', #4386, #251, #4854, .T. ) ;
#5945 = DIRECTION ( 'NONE',  ( -0.000000000000000000, -0.000000000000000000, 1.000000000000000000 ) ) ;
#5946 = AXIS2_PLACEMENT_3D ( 'NONE', #1970, #3867, #5811 ) ;
#5947 = CARTESIAN_POINT ( 'NONE',  ( 12.24718835365690772, 4.666802875123989836, 33.22501703466258505 ) ) ;
#5948 = EDGE_CURVE ( 'NONE', #2604, #836, #1637, .T. ) ;
#5949 = CARTESIAN_POINT ( 'NONE',  ( 1.131281550719567528E-13, 1.761763928569687004E-14, -35.00000000000000000 ) ) ;
#5950 = ORIENTED_EDGE ( 'NONE', *, *, #2427, .F. ) ;
#5951 = ORIENTED_EDGE ( 'NONE', *, *, #5944, .F. ) ;
#5952 = CIRCLE ( 'NONE', #794, 5.000000000000004441 ) ;
#5953 = CARTESIAN_POINT ( 'NONE',  ( -0.8304760625349921765, -8.965668681055127820, 23.09216300389308074 ) ) ;
#5954 = EDGE_CURVE ( 'NONE', #2204, #4527, #1000, .T. ) ;
#5955 = EDGE_LOOP ( 'NONE', ( #1377, #5409, #2909, #6129, #6097, #5513, #3313, #5641, #4012 ) ) ;
#5956 = DIRECTION ( 'NONE',  ( -1.000000000000000000, 0.000000000000000000, 0.000000000000000000 ) ) ;
#5957 = CIRCLE ( 'NONE', #5362, 9.999999999999996447 ) ;
#5958 = EDGE_LOOP ( 'NONE', ( #1514, #5336, #1443, #5980, #3268, #3375, #734 ) ) ;
#5959 = CARTESIAN_POINT ( 'NONE',  ( 11.82353433160560385, -71.60642589802972680, 35.00000000000000000 ) ) ;
#5960 = LINE ( 'NONE', #4423, #2570 ) ;
#5961 = CIRCLE ( 'NONE', #2760, 5.000000000000003553 ) ;
#5962 = DIRECTION ( 'NONE',  ( -0.000000000000000000, -0.000000000000000000, -1.000000000000000000 ) ) ;
#5963 = FACE_OUTER_BOUND ( 'NONE', #3808, .T. ) ;
#5964 = AXIS2_PLACEMENT_3D ( 'NONE', #741, #1142, #1679 ) ;
#5965 = ORIENTED_EDGE ( 'NONE', *, *, #3350, .F. ) ;
#5966 = CARTESIAN_POINT ( 'NONE',  ( 9.157688896001753065, 8.975362584346067152, 22.85246612729342885 ) ) ;
#5967 = CIRCLE ( 'NONE', #511, 9.999999999999992895 ) ;
#5968 = LINE ( 'NONE', #3093, #5639 ) ;
#5969 = DIRECTION ( 'NONE',  ( 0.5000000000000103251, -0.8660254037844326014, 0.000000000000000000 ) ) ;
#5970 = ORIENTED_EDGE ( 'NONE', *, *, #777, .F. ) ;
#5971 = DIRECTION ( 'NONE',  ( 0.7071067811865464625, -0.7071067811865486830, 0.000000000000000000 ) ) ;
#5972 = CARTESIAN_POINT ( 'NONE',  ( -12.41448144607148230, 6.563799387313612677, 35.72511331161845050 ) ) ;
#5973 = APPLICATION_CONTEXT ( 'automotive_design' ) ;
#5974 = EDGE_LOOP ( 'NONE', ( #980, #3091, #902, #602 ) ) ;
#5975 = CARTESIAN_POINT ( 'NONE',  ( -9.994658916190591214, 8.983694681928700021, 22.80938439471025703 ) ) ;
#5976 = CARTESIAN_POINT ( 'NONE',  ( -5.000000000000003553, 89.46264649666795776, -79.99999999999998579 ) ) ;
#5977 = CARTESIAN_POINT ( 'NONE',  ( -80.08403291566554572, 27.64547812922971914, 40.00000000000000000 ) ) ;
#5978 = CARTESIAN_POINT ( 'NONE',  ( 12.00000000000000000, 0.000000000000000000, 20.00000000000000000 ) ) ;
#5979 = CARTESIAN_POINT ( 'NONE',  ( -5.114554293134481958E-14, -6.349488965209747807E-14, -35.00000000000000000 ) ) ;
#5980 = ORIENTED_EDGE ( 'NONE', *, *, #698, .F. ) ;
#5981 = CARTESIAN_POINT ( 'NONE',  ( -8.069545871843429197, 13.47611570251764590, 37.99999999999999289 ) ) ;
#5982 = EDGE_CURVE ( 'NONE', #4796, #5277, #5750, .T. ) ;
#5983 = CARTESIAN_POINT ( 'NONE',  ( 1.660911000355770106, -8.965240827029075987, 23.08598180255752297 ) ) ;
#5984 = ORIENTED_EDGE ( 'NONE', *, *, #1847, .F. ) ;
#5985 = CARTESIAN_POINT ( 'NONE',  ( -8.999999999999996447, 6.000548030722253401, 23.13502304888919170 ) ) ;
#5986 = ORIENTED_EDGE ( 'NONE', *, *, #5791, .F. ) ;
#5987 = DIRECTION ( 'NONE',  ( 0.5000000000000081046, -0.8660254037844340447, 0.000000000000000000 ) ) ;
#5988 = DIRECTION ( 'NONE',  ( -1.000000000000000000, 0.000000000000000000, 0.000000000000000000 ) ) ;
#5989 = CARTESIAN_POINT ( 'NONE',  ( 5.114554293134526134E-14, 6.349488965209711204E-14, 35.00000000000000000 ) ) ;
#5990 = EDGE_CURVE ( 'NONE', #1698, #2290, #2840, .T. ) ;
#5991 = CARTESIAN_POINT ( 'NONE',  ( -9.999999999999998224, 4.166666666666706931, 23.00000000000000000 ) ) ;
#5992 = DIRECTION ( 'NONE',  ( 8.673617379883998001E-16, 1.000000000000000000, 0.000000000000000000 ) ) ;
#5993 = DIRECTION ( 'NONE',  ( -1.000000000000000000, 0.000000000000000000, 0.000000000000000000 ) ) ;
#5994 = CARTESIAN_POINT ( 'NONE',  ( -3.785572473853681785, 14.18798205797855694, 38.16905032409690790 ) ) ;
#5995 = FACE_OUTER_BOUND ( 'NONE', #4864, .T. ) ;
#5996 = VERTEX_POINT ( 'NONE', #2976 ) ;
#5997 = CARTESIAN_POINT ( 'NONE',  ( 13.68733454931619775, -1.968046268140574151, 35.80501179064256689 ) ) ;
#5998 = CARTESIAN_POINT ( 'NONE',  ( -10.63625351335941893, 9.632247231687291134, 35.59852902770369099 ) ) ;
#5999 = ORIENTED_EDGE ( 'NONE', *, *, #1222, .T. ) ;
#6000 = CARTESIAN_POINT ( 'NONE',  ( -9.419333092092999848, 9.933255351449997050, 30.50691708577705796 ) ) ;
#6001 = CARTESIAN_POINT ( 'NONE',  ( 68.69027832783777399, 26.57196568621521138, -35.00000000000000000 ) ) ;
#6002 = ADVANCED_FACE ( 'NONE', ( #2414 ), #5132, .T. ) ;
#6003 = DIRECTION ( 'NONE',  ( -8.673617379884026597E-16, 1.000000000000000000, 0.000000000000000000 ) ) ;
#6004 = DIRECTION ( 'NONE',  ( 1.000000000000000000, 0.000000000000000000, -0.000000000000000000 ) ) ;
#6005 = FACE_OUTER_BOUND ( 'NONE', #6061, .T. ) ;
#6006 = CARTESIAN_POINT ( 'NONE',  ( -8.785766938566927919, -10.67320828294309898, 33.09220912812762094 ) ) ;
#6007 = ORIENTED_EDGE ( 'NONE', *, *, #5826, .F. ) ;
#6008 = DIRECTION ( 'NONE',  ( 0.000000000000000000, -0.000000000000000000, -1.000000000000000000 ) ) ;
#6009 = ORIENTED_EDGE ( 'NONE', *, *, #3653, .F. ) ;
#6010 = DIRECTION ( 'NONE',  ( 0.8660254037844339337, 0.5000000000000079936, 0.000000000000000000 ) ) ;
#6011 = EDGE_CURVE ( 'NONE', #2727, #1135, #3334, .T. ) ;
#6012 = EDGE_CURVE ( 'NONE', #3856, #2123, #677, .T. ) ;
#6013 = DIRECTION ( 'NONE',  ( 1.000000000000000000, 0.000000000000000000, 0.000000000000000000 ) ) ;
#6014 = CONTEXT_DEPENDENT_SHAPE_REPRESENTATION ( #3212, #4939 ) ;
#6015 = CARTESIAN_POINT ( 'NONE',  ( 0.000000000000000000, 0.000000000000000000, -40.00000000000000000 ) ) ;
#6016 = CARTESIAN_POINT ( 'NONE',  ( -9.910574073276151807, 3.317157231508650828, 22.73823205004162418 ) ) ;
#6017 = DIRECTION ( 'NONE',  ( 1.000000000000000000, 0.000000000000000000, 0.000000000000000000 ) ) ;
#6018 = AXIS2_PLACEMENT_3D ( 'NONE', #3537, #4534, #704 ) ;
#6019 = ORIENTED_EDGE ( 'NONE', *, *, #3795, .T. ) ;
#6020 = DIRECTION ( 'NONE',  ( 0.3607836771741465554, 0.9326495259660518844, -0.000000000000000000 ) ) ;
#6021 = EDGE_CURVE ( 'NONE', #5794, #670, #2943, .T. ) ;
#6022 = DIRECTION ( 'NONE',  ( 0.000000000000000000, 0.000000000000000000, 1.000000000000000000 ) ) ;
#6023 = CARTESIAN_POINT ( 'NONE',  ( -9.074396217167327805, 58.26942451214400620, 35.00000000000000000 ) ) ;
#6024 = AXIS2_PLACEMENT_3D ( 'NONE', #3589, #3035, #699 ) ;
#6025 = PRESENTATION_LAYER_ASSIGNMENT (  '', '', ( #2545 ) ) ;
#6026 = CARTESIAN_POINT ( 'NONE',  ( 9.638809502600501844, -5.954811582427137040, 25.54535933516314117 ) ) ;
#6027 = AXIS2_PLACEMENT_3D ( 'NONE', #4725, #5695, #3715 ) ;
#6028 = CARTESIAN_POINT ( 'NONE',  ( -9.638809502600501844, 5.954811582427136152, 25.54535933516314472 ) ) ;
#6029 = VECTOR ( 'NONE', #4238, 1000.000000000000000 ) ;
#6030 = ORIENTED_EDGE ( 'NONE', *, *, #2746, .F. ) ;
#6031 = ADVANCED_FACE ( 'NONE', ( #3610 ), #1205, .T. ) ;
#6032 = CARTESIAN_POINT ( 'NONE',  ( -4.399300199984973681, 10.59948853791303947, 28.13666499103235097 ) ) ;
#6033 = DIRECTION ( 'NONE',  ( 1.000000000000000000, 0.000000000000000000, 0.000000000000000000 ) ) ;
#6034 = PRODUCT_DEFINITION_SHAPE ( 'NONE', 'NONE',  #2300 ) ;
#6035 = DIRECTION ( 'NONE',  ( -0.9880900209011910240, 0.1538769332794358846, 0.000000000000000000 ) ) ;
#6036 = DIRECTION ( 'NONE',  ( -0.000000000000000000, -0.000000000000000000, -1.000000000000000000 ) ) ;
#6037 = AXIS2_PLACEMENT_3D ( 'NONE', #3597, #205, #5956 ) ;
#6038 = DIRECTION ( 'NONE',  ( 0.9880900209011891366, 0.1538769332794488465, -0.000000000000000000 ) ) ;
#6039 = DIRECTION ( 'NONE',  ( -1.000000000000000000, 0.000000000000000000, 0.000000000000000000 ) ) ;
#6040 = VECTOR ( 'NONE', #3927, 1000.000000000000000 ) ;
#6041 = ORIENTED_EDGE ( 'NONE', *, *, #2439, .F. ) ;
#6042 = DIRECTION ( 'NONE',  ( 1.000000000000000000, 0.000000000000000000, 0.000000000000000000 ) ) ;
#6043 = ORIENTED_EDGE ( 'NONE', *, *, #6065, .F. ) ;
#6044 = DIRECTION ( 'NONE',  ( 0.000000000000000000, 0.000000000000000000, 1.000000000000000000 ) ) ;
#6045 = CARTESIAN_POINT ( 'NONE',  ( 62.30180741492871022, 50.18450749816254586, -35.00000000000000000 ) ) ;
#6046 = CONTEXT_DEPENDENT_SHAPE_REPRESENTATION ( #1725, #1386 ) ;
#6047 = VECTOR ( 'NONE', #4765, 999.9999999999998863 ) ;
#6048 = DIRECTION ( 'NONE',  ( 1.000000000000000000, 0.000000000000000000, 0.000000000000000000 ) ) ;
#6049 = CARTESIAN_POINT ( 'NONE',  ( -9.999999999999998224, -8.333333333333314386, 23.00000000000000000 ) ) ;
#6050 = CARTESIAN_POINT ( 'NONE',  ( 9.000000000000005329, -8.999999999988066435, 23.06137295785747554 ) ) ;
#6051 = VECTOR ( 'NONE', #5371, 999.9999999999998863 ) ;
#6052 = VERTEX_POINT ( 'NONE', #4080 ) ;
#6053 = PLANE ( 'NONE',  #4868 ) ;
#6054 = PLANE ( 'NONE',  #2224 ) ;
#6055 = DIRECTION ( 'NONE',  ( -0.3607836771741652626, 0.9326495259660447790, 0.000000000000000000 ) ) ;
#6056 =( LENGTH_UNIT ( ) NAMED_UNIT ( * ) SI_UNIT ( .MILLI., .METRE. ) );
#6057 = CARTESIAN_POINT ( 'NONE',  ( 8.964680801521355491, -2.491918585145489029, 23.07363600708416129 ) ) ;
#6058 = ADVANCED_FACE ( 'NONE', ( #4492 ), #245, .F. ) ;
#6059 = CARTESIAN_POINT ( 'NONE',  ( -11.22195964661421819, 5.390571672161876826, 30.65936073406735574 ) ) ;
#6060 = CIRCLE ( 'NONE', #4155, 5.000000000000003553 ) ;
#6061 = EDGE_LOOP ( 'NONE', ( #1148, #4882, #1127, #260 ) ) ;
#6062 = CARTESIAN_POINT ( 'NONE',  ( -5.819383256046894992, 8.963566061094550008, 22.99383858586042351 ) ) ;
#6063 = PLANE ( 'NONE',  #5231 ) ;
#6064 = DIRECTION ( 'NONE',  ( 0.000000000000000000, 0.000000000000000000, 1.000000000000000000 ) ) ;
#6065 = EDGE_CURVE ( 'NONE', #2500, #6095, #5437, .T. ) ;
#6066 = DIRECTION ( 'NONE',  ( -0.000000000000000000, -0.000000000000000000, -1.000000000000000000 ) ) ;
#6067 = DIRECTION ( 'NONE',  ( -0.000000000000000000, -0.000000000000000000, -1.000000000000000000 ) ) ;
#6068 = CARTESIAN_POINT ( 'NONE',  ( -10.13908112636436343, -9.618700053625529378, 30.46372964425718521 ) ) ;
#6069 = ORIENTED_EDGE ( 'NONE', *, *, #392, .T. ) ;
#6070 = PLANE ( 'NONE',  #1471 ) ;
#6071 = VERTEX_POINT ( 'NONE', #1256 ) ;
#6072 = CARTESIAN_POINT ( 'NONE',  ( 11.50000000000000178, 67.50000000000000000, -20.00000000000000000 ) ) ;
#6073 = CARTESIAN_POINT ( 'NONE',  ( -9.192833548570002122, 59.02994620156853500, -35.00000000000000000 ) ) ;
#6074 = CARTESIAN_POINT ( 'NONE',  ( 0.000000000000000000, 0.000000000000000000, -35.00000000000000000 ) ) ;
#6075 = CARTESIAN_POINT ( 'NONE',  ( -12.35760627049922178, 9.696021465980074083, 38.00000000000000000 ) ) ;
#6076 = LINE ( 'NONE', #3639, #3259 ) ;
#6077 = EDGE_CURVE ( 'NONE', #5369, #4004, #868, .T. ) ;
#6078 = ORIENTED_EDGE ( 'NONE', *, *, #285, .F. ) ;
#6079 = CYLINDRICAL_SURFACE ( 'NONE', #4244, 5.000000000000004441 ) ;
#6080 = CARTESIAN_POINT ( 'NONE',  ( -9.500000000000008882, 67.50000000000000000, -20.00000000000000000 ) ) ;
#6081 = CARTESIAN_POINT ( 'NONE',  ( -1.301042606982566193E-13, 14.99999999999956124, -35.00000000000000000 ) ) ;
#6082 = CARTESIAN_POINT ( 'NONE',  ( 9.908812100099982700, 1.716690548177159270, 25.63028262842344773 ) ) ;
#6083 = CARTESIAN_POINT ( 'NONE',  ( -14.42236408824967775, 3.019346778933466258, 38.33740271606986738 ) ) ;
#6084 = VERTEX_POINT ( 'NONE', #275 ) ;
#6085 = CARTESIAN_POINT ( 'NONE',  ( -6.563632016262921809, 12.41454131244163861, 35.72510948639917672 ) ) ;
#6086 = CYLINDRICAL_SURFACE ( 'NONE', #371, 80.00000000000000000 ) ;
#6087 = ADVANCED_FACE ( 'NONE', ( #5995 ), #3094, .F. ) ;
#6088 = EDGE_CURVE ( 'NONE', #4900, #3566, #5937, .T. ) ;
#6089 = ORIENTED_EDGE ( 'NONE', *, *, #1662, .T. ) ;
#6090 = CYLINDRICAL_SURFACE ( 'NONE', #2039, 15.67638808697555142 ) ;
#6091 = DIRECTION ( 'NONE',  ( 1.000000000000000000, 0.000000000000000000, 0.000000000000000000 ) ) ;
#6092 = LINE ( 'NONE', #1908, #466 ) ;
#6093 = EDGE_CURVE ( 'NONE', #936, #2868, #2042, .T. ) ;
#6094 = CARTESIAN_POINT ( 'NONE',  ( -10.27356722921338950, -10.12138240269938727, 35.55812462721154787 ) ) ;
#6095 = VERTEX_POINT ( 'NONE', #746 ) ;
#6096 = LINE ( 'NONE', #2203, #2368 ) ;
#6097 = ORIENTED_EDGE ( 'NONE', *, *, #2631, .F. ) ;
#6098 = FACE_OUTER_BOUND ( 'NONE', #4745, .T. ) ;
#6099 = ADVANCED_FACE ( 'NONE', ( #188 ), #4047, .F. ) ;
#6100 = DIRECTION ( 'NONE',  ( -0.000000000000000000, -0.000000000000000000, -1.000000000000000000 ) ) ;
#6101 = CONTEXT_DEPENDENT_SHAPE_REPRESENTATION ( #1936, #2090 ) ;
#6102 = DIRECTION ( 'NONE',  ( 0.7071067811865486830, 0.7071067811865464625, -0.000000000000000000 ) ) ;
#6103 = ORIENTED_EDGE ( 'NONE', *, *, #6065, .T. ) ;
#6104 = CARTESIAN_POINT ( 'NONE',  ( -9.969668718019493170, 9.144590365090033757, 22.73823205004162418 ) ) ;
#6105 = DIRECTION ( 'NONE',  ( -0.000000000000000000, 0.000000000000000000, 1.000000000000000000 ) ) ;
#6106 = ORIENTED_EDGE ( 'NONE', *, *, #21, .F. ) ;
#6107 = CARTESIAN_POINT ( 'NONE',  ( -9.999999999999998224, -9.999999999999998224, -167.0000000000000284 ) ) ;
#6108 = CARTESIAN_POINT ( 'NONE',  ( -12.31015466235523981, 79.04720167209522685, 35.00000000000000000 ) ) ;
#6109 = CARTESIAN_POINT ( 'NONE',  ( -67.15076586955525784, -25.97642475653991312, 45.00000000000000711 ) ) ;
#6110 = ADVANCED_BREP_SHAPE_REPRESENTATION ( '', ( #2173, #73 ), #2452 ) ;
#6111 = LINE ( 'NONE', #4806, #3563 ) ;
#6112 = CARTESIAN_POINT ( 'NONE',  ( 11.69030472852371005, -2.742560498089769982, 30.70728637550628903 ) ) ;
#6113 = FILL_AREA_STYLE ('',( #3249 ) ) ;
#6114 = ORIENTED_EDGE ( 'NONE', *, *, #4966, .T. ) ;
#6115 = CARTESIAN_POINT ( 'NONE',  ( -3.759289558891020455, 12.45812449473958949, 33.24069098933200195 ) ) ;
#6116 = ORIENTED_EDGE ( 'NONE', *, *, #818, .T. ) ;
#6117 = LINE ( 'NONE', #5591, #5842 ) ;
#6118 = CONICAL_SURFACE ( 'NONE', #2725, 80.99999999999998579, 0.7853981633974482790 ) ;
#6119 = VERTEX_POINT ( 'NONE', #4554 ) ;
#6120 = DIRECTION ( 'NONE',  ( 0.5000000000000099920, -0.8660254037844328234, 0.000000000000000000 ) ) ;
#6121 = VECTOR ( 'NONE', #1353, 1000.000000000000000 ) ;
#6122 = EDGE_CURVE ( 'NONE', #3175, #3262, #5540, .T. ) ;
#6123 = FACE_OUTER_BOUND ( 'NONE', #947, .T. ) ;
#6124 = AXIS2_PLACEMENT_3D ( 'NONE', #5849, #89, #3002 ) ;
#6125 = EDGE_CURVE ( 'NONE', #2223, #5916, #3627, .T. ) ;
#6126 = CARTESIAN_POINT ( 'NONE',  ( 9.166555234036119160, 10.04707028972859106, 25.36260747786040071 ) ) ;
#6127 = VERTEX_POINT ( 'NONE', #3965 ) ;
#6128 = CARTESIAN_POINT ( 'NONE',  ( -11.08488032081242025, 11.08488032081242203, 38.00000000000000000 ) ) ;
#6129 = ORIENTED_EDGE ( 'NONE', *, *, #3841, .F. ) ;
#6130 = CARTESIAN_POINT ( 'NONE',  ( 12.49999999999999822, 67.50000000000000000, 19.00000000000001066 ) ) ;
#6131 =( GEOMETRIC_REPRESENTATION_CONTEXT ( 3 ) GLOBAL_UNCERTAINTY_ASSIGNED_CONTEXT ( ( #4688 ) ) GLOBAL_UNIT_ASSIGNED_CONTEXT ( ( #5652, #550, #5835 ) ) REPRESENTATION_CONTEXT ( 'NONE', 'WORKASPACE' ) );
#6132 = FACE_OUTER_BOUND ( 'NONE', #525, .T. ) ;
#6133 = DIRECTION ( 'NONE',  ( 0.7071067811865474617, 0.000000000000000000, 0.7071067811865474617 ) ) ;
#6134 = VERTEX_POINT ( 'NONE', #1620 ) ;
#6135 = FACE_BOUND ( 'NONE', #5548, .T. ) ;
#6136 = EDGE_CURVE ( 'NONE', #3527, #5318, #964, .T. ) ;
#6137 = CARTESIAN_POINT ( 'NONE',  ( 15.00000000000000000, 50.91502622129181788, -20.00000000000000000 ) ) ;
#6138 = ORIENTED_EDGE ( 'NONE', *, *, #848, .F. ) ;
#6139 = ORIENTED_EDGE ( 'NONE', *, *, #5759, .T. ) ;
#6140 = CARTESIAN_POINT ( 'NONE',  ( -11.03292118881348216, -8.007183658747740296, 33.12420745160152080 ) ) ;
#6141 = NEXT_ASSEMBLY_USAGE_OCCURRENCE ( 'NAUO1', ' ', ' ', #2300, #313, $ ) ;
#6142 = NEXT_ASSEMBLY_USAGE_OCCURRENCE ( 'NAUO2', ' ', ' ', #2300, #2955, $ ) ;
#6143 = NEXT_ASSEMBLY_USAGE_OCCURRENCE ( 'NAUO3', ' ', ' ', #2300, #1387, $ ) ;
#6144 = NEXT_ASSEMBLY_USAGE_OCCURRENCE ( 'NAUO4', ' ', ' ', #2300, #5093, $ ) ;
#6145 = NEXT_ASSEMBLY_USAGE_OCCURRENCE ( 'NAUO5', ' ', ' ', #2300, #118, $ ) ;
#6146 = NEXT_ASSEMBLY_USAGE_OCCURRENCE ( 'NAUO6', ' ', ' ', #2300, #2955, $ ) ;
#6147 = NEXT_ASSEMBLY_USAGE_OCCURRENCE ( 'NAUO7', ' ', ' ', #2300, #2955, $ ) ;
#6148 = NEXT_ASSEMBLY_USAGE_OCCURRENCE ( 'NAUO8', ' ', ' ', #2300, #2955, $ ) ;
#6149 = NEXT_ASSEMBLY_USAGE_OCCURRENCE ( 'NAUO9', ' ', ' ', #2300, #2955, $ ) ;
#6150 = NEXT_ASSEMBLY_USAGE_OCCURRENCE ( 'NAUO10', ' ', ' ', #2300, #2955, $ ) ;
#6151 = NEXT_ASSEMBLY_USAGE_OCCURRENCE ( 'NAUO11', ' ', ' ', #2300, #5093, $ ) ;
#6152 = NEXT_ASSEMBLY_USAGE_OCCURRENCE ( 'NAUO12', ' ', ' ', #2300, #1387, $ ) ;
#6153 = NEXT_ASSEMBLY_USAGE_OCCURRENCE ( 'NAUO13', ' ', ' ', #2300, #1387, $ ) ;
#6154 = NEXT_ASSEMBLY_USAGE_OCCURRENCE ( 'NAUO14', ' ', ' ', #2300, #1387, $ ) ;
#6155 = NEXT_ASSEMBLY_USAGE_OCCURRENCE ( 'NAUO15', ' ', ' ', #2300, #5093, $ ) ;
#6156 = NEXT_ASSEMBLY_USAGE_OCCURRENCE ( 'NAUO16', ' ', ' ', #2300, #5093, $ ) ;
#6157=COLOUR_RGB('Dark Blue',0.08,0.2,0.34);
#6158=FILL_AREA_STYLE_COLOUR('',#6157);
#6159=FILL_AREA_STYLE('',(#6158));
#6160=SURFACE_STYLE_FILL_AREA(#6159);
#6161=SURFACE_SIDE_STYLE('',(#6160));
#6162=SURFACE_STYLE_USAGE(.BOTH.,#6161);
#6163=PRESENTATION_STYLE_ASSIGNMENT((#6162));
#6164=COLOUR_RGB('Light Blue',0.38,0.62,0.78);
#6165=FILL_AREA_STYLE_COLOUR('',#6164);
#6166=FILL_AREA_STYLE('',(#6165));
#6167=SURFACE_STYLE_FILL_AREA(#6166);
#6168=SURFACE_SIDE_STYLE('',(#6167));
#6169=SURFACE_STYLE_USAGE(.BOTH.,#6168);
#6170=PRESENTATION_STYLE_ASSIGNMENT((#6169));
#6171=COLOUR_RGB('Sky Blue',0.24,0.69,0.87);
#6172=FILL_AREA_STYLE_COLOUR('',#6171);
#6173=FILL_AREA_STYLE('',(#6172));
#6174=SURFACE_STYLE_FILL_AREA(#6173);
#6175=SURFACE_SIDE_STYLE('',(#6174));
#6176=SURFACE_STYLE_USAGE(.BOTH.,#6175);
#6177=PRESENTATION_STYLE_ASSIGNMENT((#6176));
#6178=COLOUR_RGB('Grey',0.48,0.52,0.57);
#6179=FILL_AREA_STYLE_COLOUR('',#6178);
#6180=FILL_AREA_STYLE('',(#6179));
#6181=SURFACE_STYLE_FILL_AREA(#6180);
#6182=SURFACE_SIDE_STYLE('',(#6181));
#6183=SURFACE_STYLE_USAGE(.BOTH.,#6182);
#6184=PRESENTATION_STYLE_ASSIGNMENT((#6183));
#6185=COLOUR_RGB('Black',0.12,0.14,0.17);
#6186=FILL_AREA_STYLE_COLOUR('',#6185);
#6187=FILL_AREA_STYLE('',(#6186));
#6188=SURFACE_STYLE_FILL_AREA(#6187);
#6189=SURFACE_SIDE_STYLE('',(#6188));
#6190=SURFACE_STYLE_USAGE(.BOTH.,#6189);
#6191=PRESENTATION_STYLE_ASSIGNMENT((#6190));
#6192=COLOUR_RGB('Off White',0.89,0.88,0.83);
#6193=FILL_AREA_STYLE_COLOUR('',#6192);
#6194=FILL_AREA_STYLE('',(#6193));
#6195=SURFACE_STYLE_FILL_AREA(#6194);
#6196=SURFACE_SIDE_STYLE('',(#6195));
#6197=SURFACE_STYLE_USAGE(.BOTH.,#6196);
#6198=PRESENTATION_STYLE_ASSIGNMENT((#6197));
ENDSEC;
END-ISO-10303-21;
